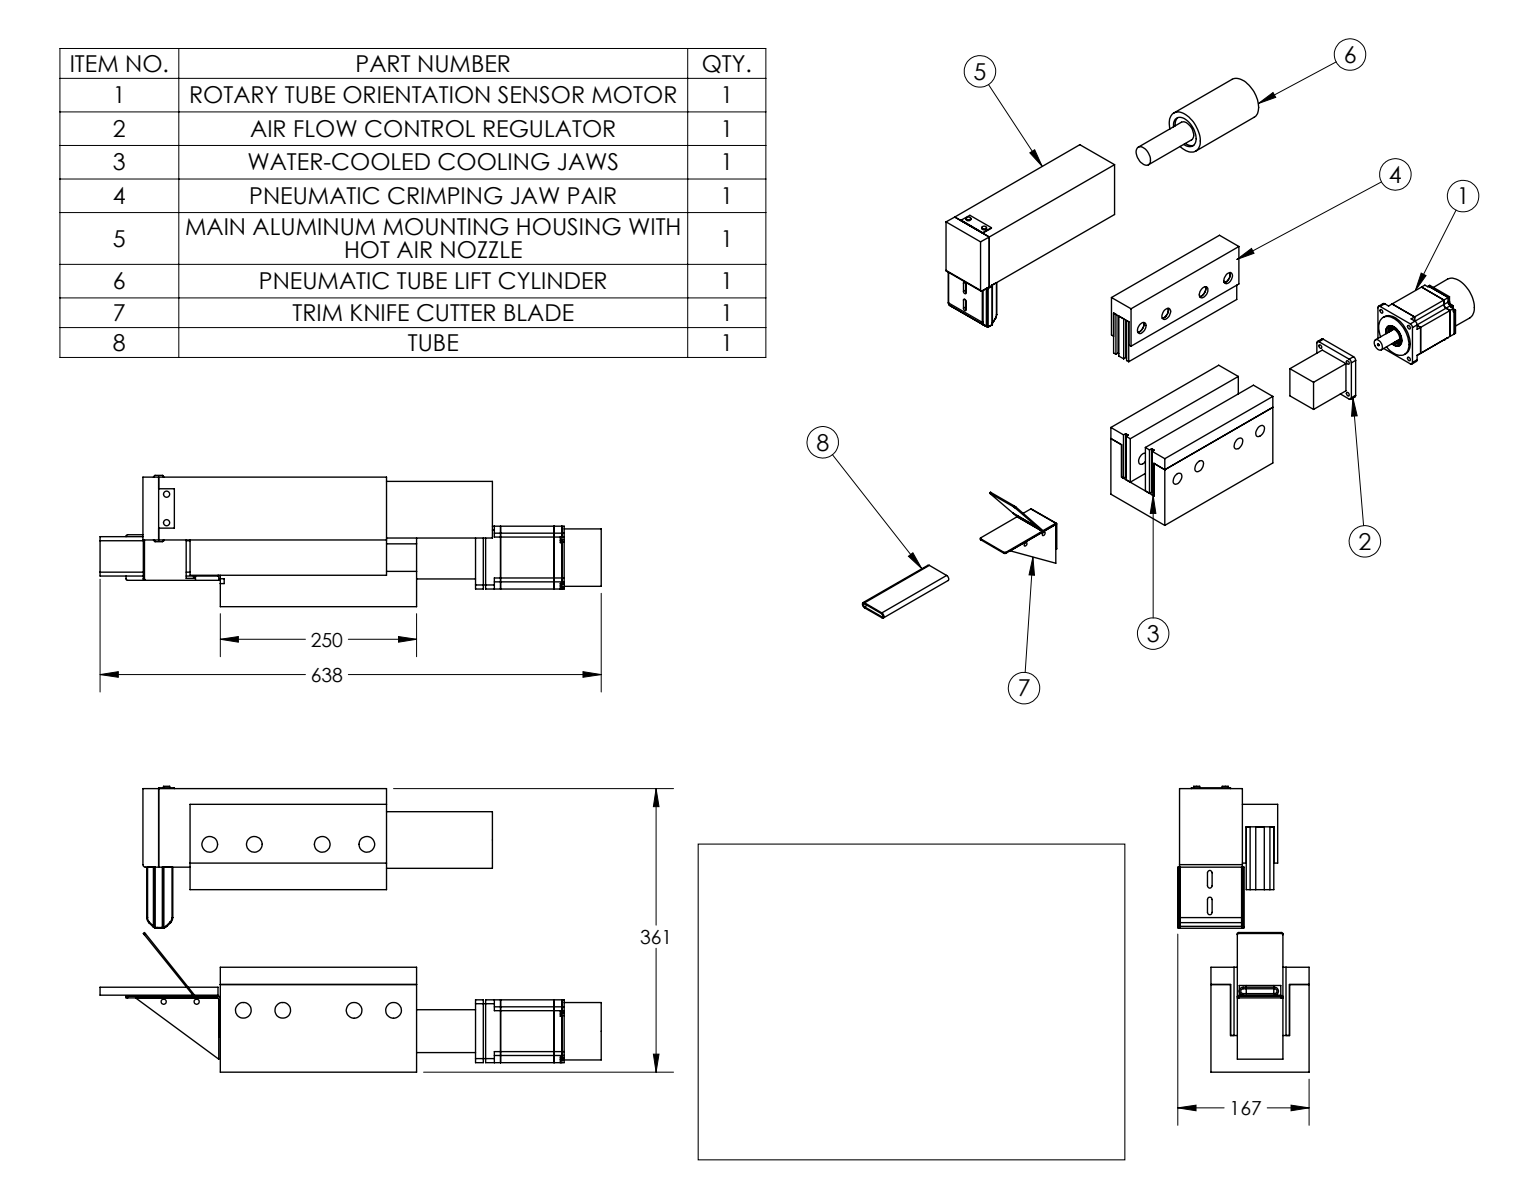
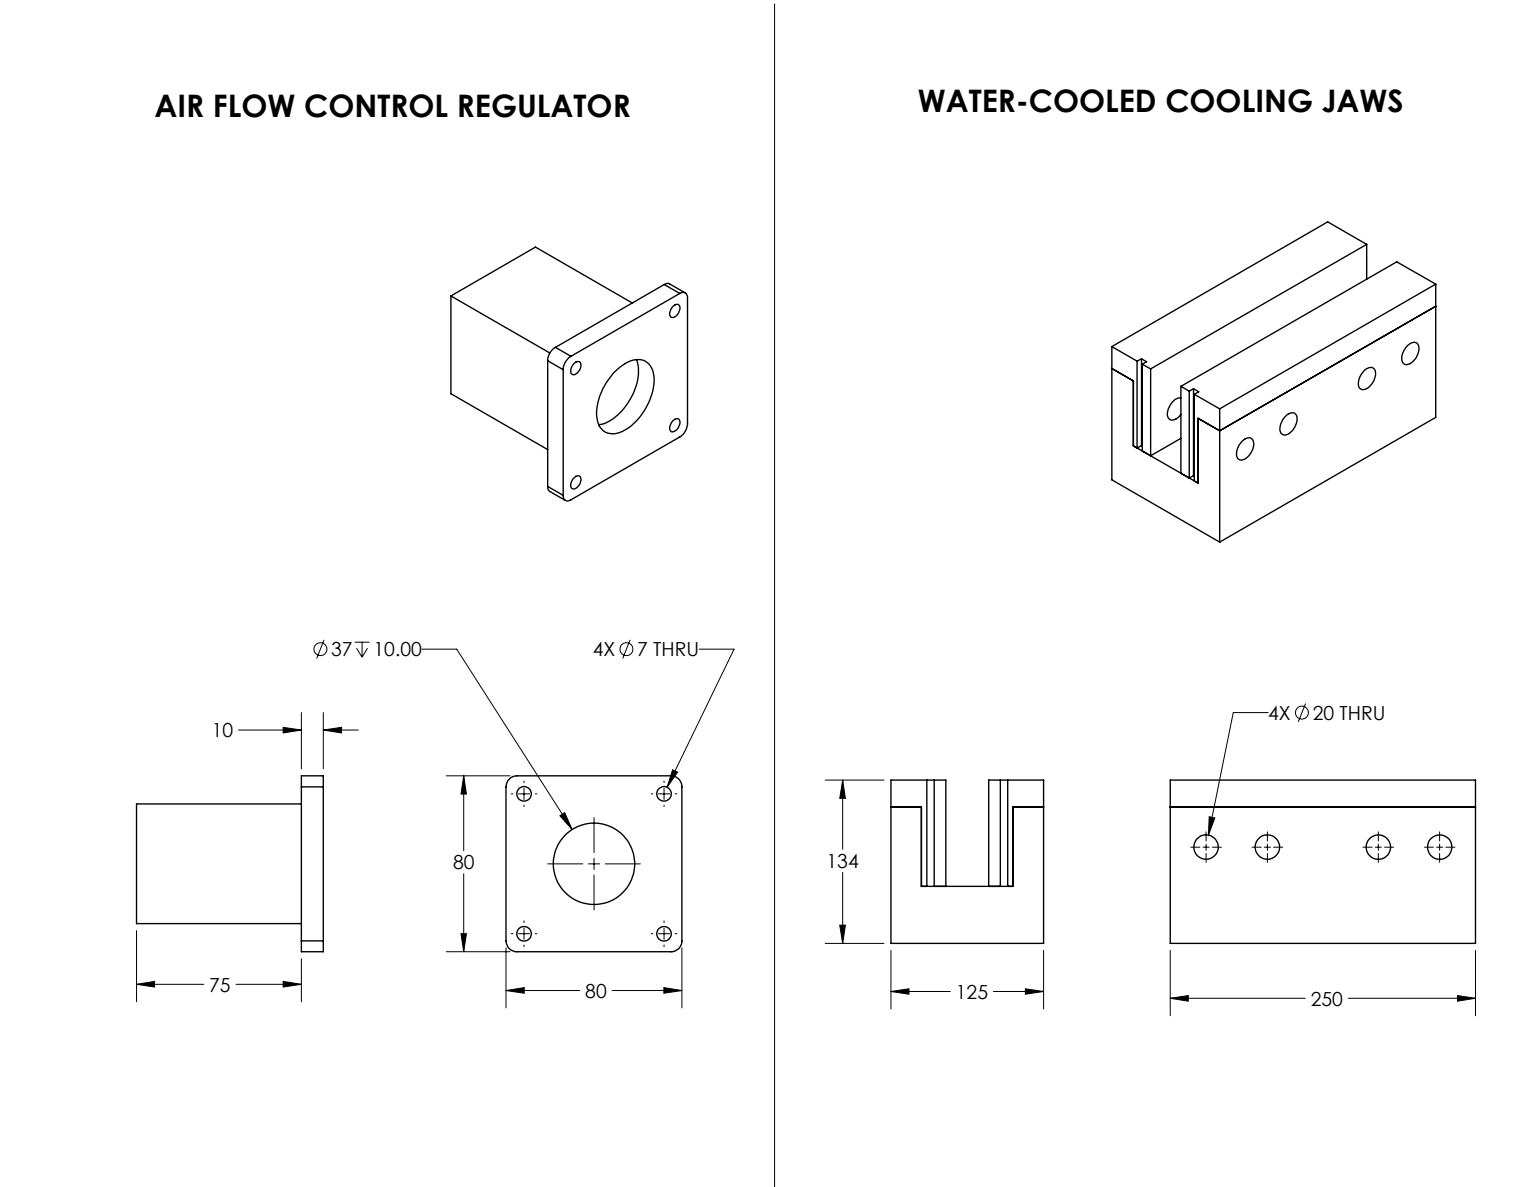
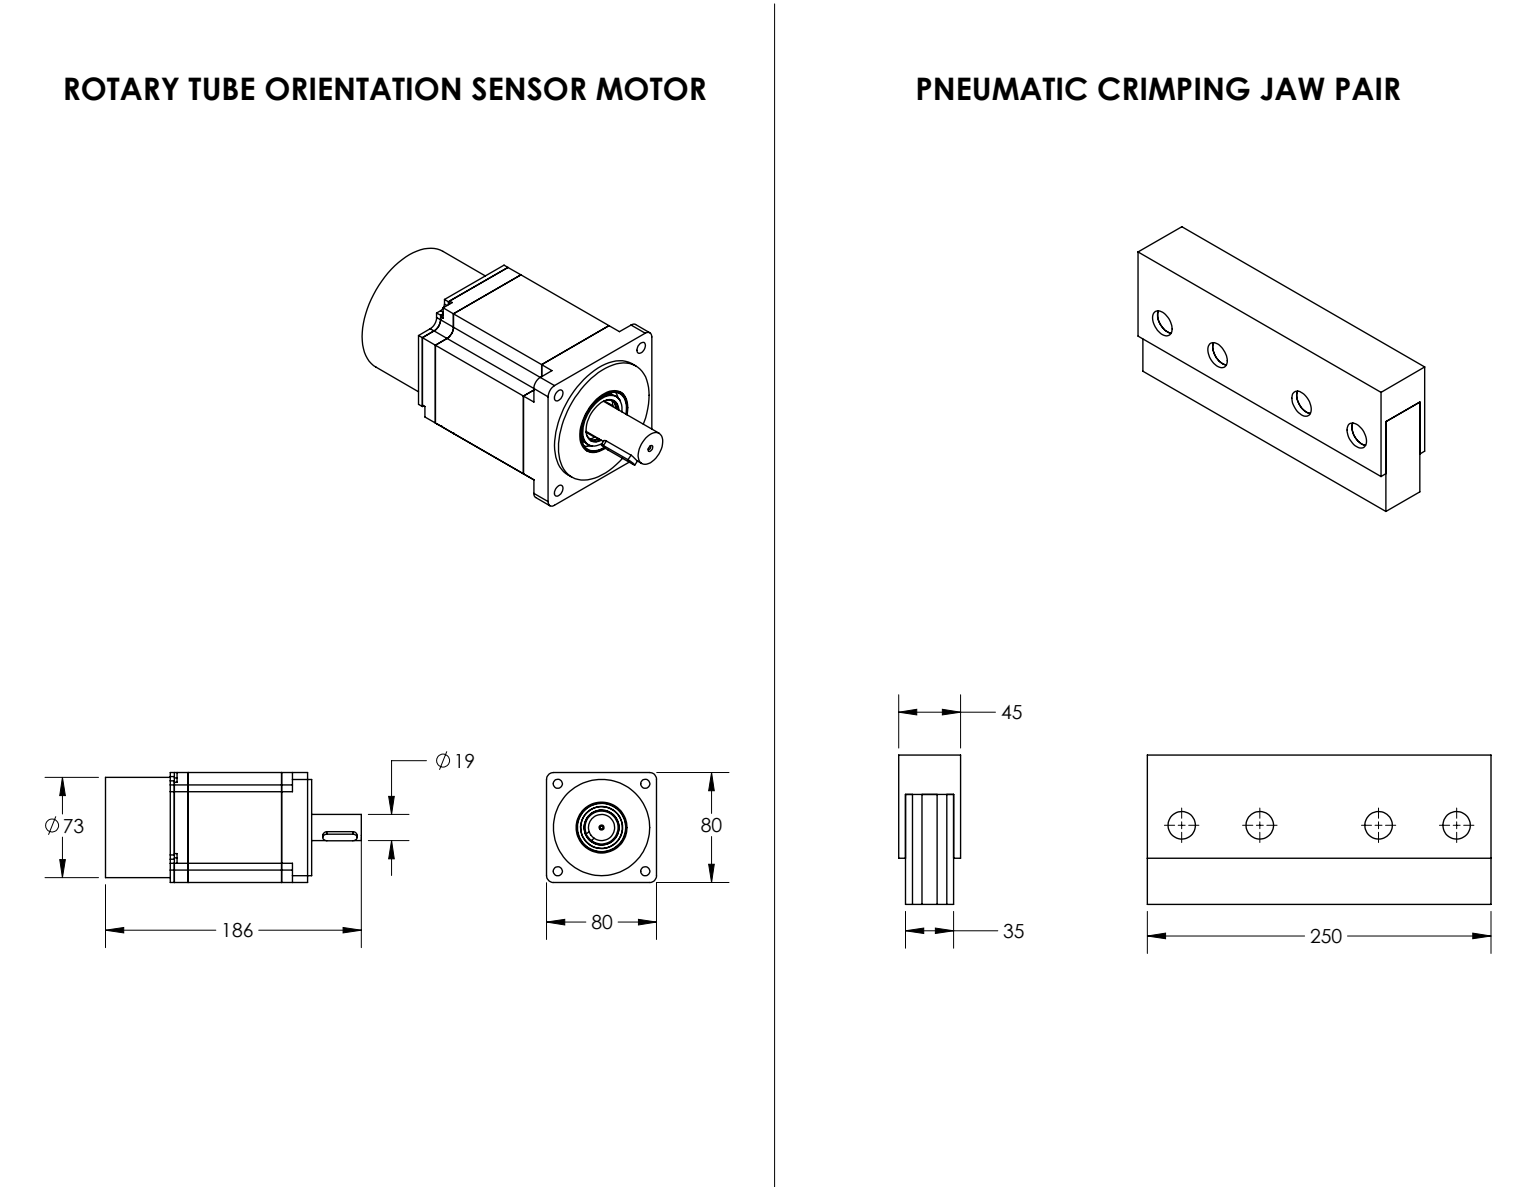
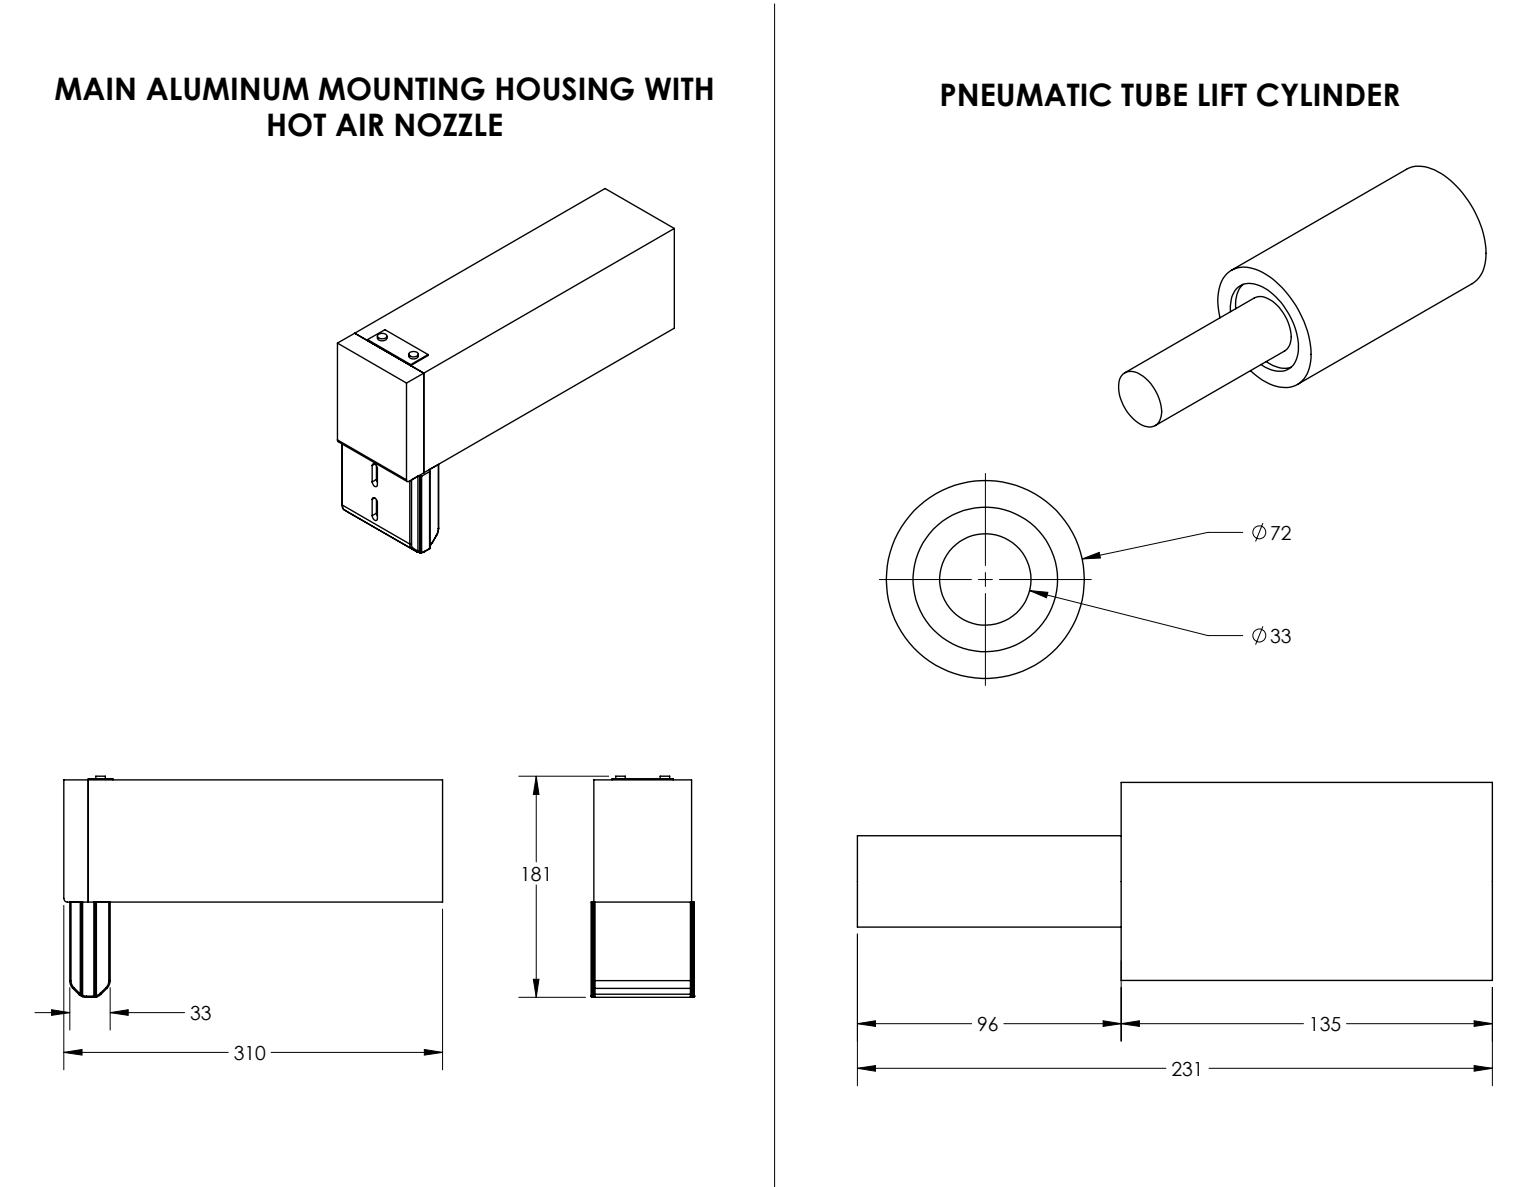
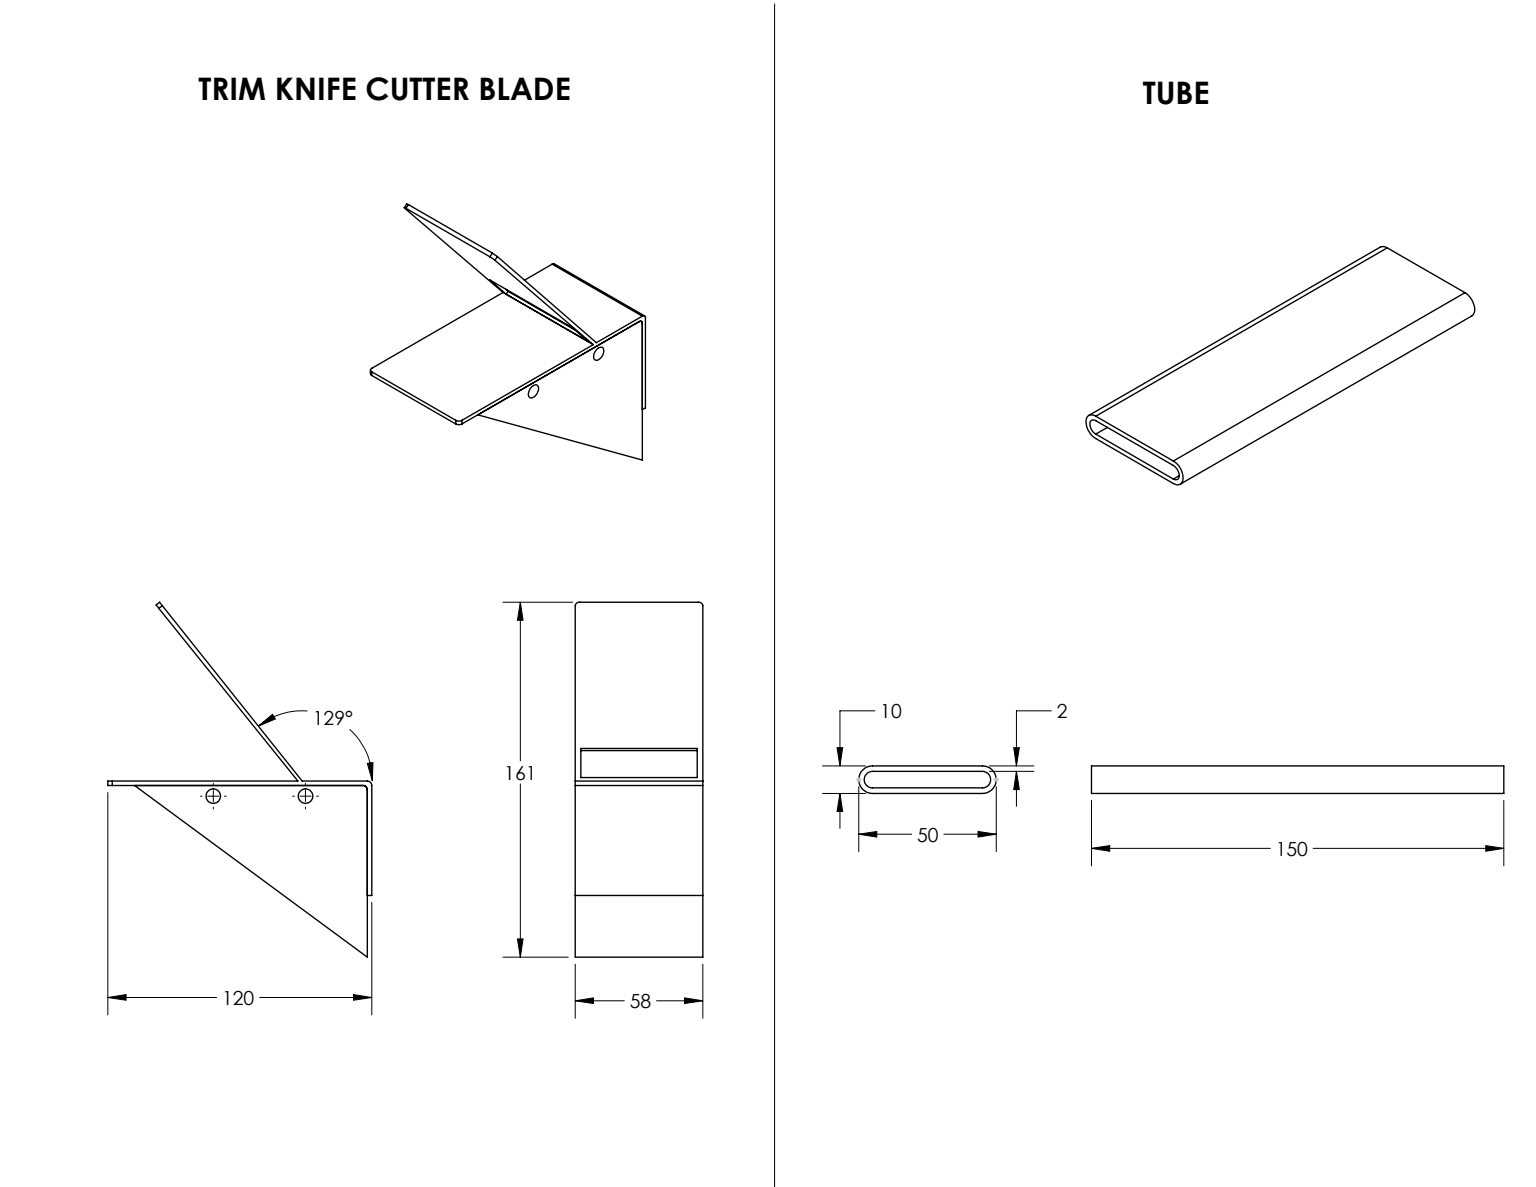
ISO-10303-21;
HEADER;
FILE_DESCRIPTION (('STEP AP214'),
    '1' );
FILE_NAME ('TAS-006',
    '2026-11-01T06:29:40',
    ( '' ),
    ( '' ),
    'SwSTEP 2.0',
    'SolidWorks 2024',
    '' );
FILE_SCHEMA (( 'AUTOMOTIVE_DESIGN' ));
ENDSEC;

DATA;
#1 = DIRECTION ( 'NONE',  ( -1.000000000000000000, 0.000000000000000000, 0.000000000000000000 ) ) ;
#2 = VECTOR ( 'NONE', #10690, 1000.000000000000000 ) ;
#3 = CARTESIAN_POINT ( 'NONE',  ( 26.00000000000000000, 19.00000000000000000, 40.00000000000001421 ) ) ;
#4 = VECTOR ( 'NONE', #1061, 1000.000000000000227 ) ;
#5 = SURFACE_STYLE_USAGE ( .BOTH. , #14117 ) ;
#6 = AXIS2_PLACEMENT_3D ( 'NONE', #11999, #10445, #9105 ) ;
#7 = DIRECTION ( 'NONE',  ( -0.000000000000000000, -0.000000000000000000, 1.000000000000000000 ) ) ;
#8 = FACE_OUTER_BOUND ( 'NONE', #1374, .T. ) ;
#9 = CARTESIAN_POINT ( 'NONE',  ( -0.9675204218459506622, 140.4913968989433499, 501.9874629796761383 ) ) ;
#10 = EDGE_CURVE ( 'NONE', #8032, #20154, #10638, .T. ) ;
#11 = ORIENTED_EDGE ( 'NONE', *, *, #4617, .F. ) ;
#12 = CARTESIAN_POINT ( 'NONE',  ( 153.4893729001366580, 145.9162550801369491, 0.000000000000000000 ) ) ;
#13 = CARTESIAN_POINT ( 'NONE',  ( 498.8334540492693918, 191.8198460455371333, 24.99421986894476078 ) ) ;
#14 = VECTOR ( 'NONE', #3072, 1000.000000000000000 ) ;
#15 = VECTOR ( 'NONE', #3910, 1000.000000000000000 ) ;
#16 = ORIENTED_EDGE ( 'NONE', *, *, #4980, .F. ) ;
#17 = DIRECTION ( 'NONE',  ( 0.000000000000000000, 1.000000000000000000, 0.000000000000000000 ) ) ;
#18 = ORIENTED_EDGE ( 'NONE', *, *, #2305, .F. ) ;
#19 = ADVANCED_FACE ( 'NONE', ( #19045 ), #8159, .F. ) ;
#20 = LINE ( 'NONE', #3221, #19065 ) ;
#21 = VERTEX_POINT ( 'NONE', #6304 ) ;
#22 = DIRECTION ( 'NONE',  ( 6.123031769111888756E-17, -1.000000000000000000, -3.749151804555344967E-33 ) ) ;
#23 = CARTESIAN_POINT ( 'NONE',  ( 143.0892156028631348, 80.91625508013694912, 245.0000000000000000 ) ) ;
#24 = CARTESIAN_POINT ( 'NONE',  ( -79.99999999999995737, 146.1184945051221575, 507.7561228916242158 ) ) ;
#25 = COLOUR_RGB ( '', 0.66274510, 0.83137255, 0.94901961) ;
#26 = CARTESIAN_POINT ( 'NONE',  ( 0.7168072523057583689, 140.4381783004008355, 500.8620105408696759 ) ) ;
#27 = STYLED_ITEM ( 'NONE', ( #13030 ), #7501 ) ;
#28 = CARTESIAN_POINT ( 'NONE',  ( -20.99999999999999645, 19.00000000000000000, -35.00000000000000711 ) ) ;
#29 = FACE_OUTER_BOUND ( 'NONE', #7471, .T. ) ;
#30 = EDGE_LOOP ( 'NONE', ( #17884, #17618, #18763, #13200 ) ) ;
#31 = FACE_OUTER_BOUND ( 'NONE', #2574, .T. ) ;
#32 = CARTESIAN_POINT ( 'NONE',  ( -211.5106270998635409, 123.1299228374912644, 29.36128450348865471 ) ) ;
#33 = SURFACE_STYLE_FILL_AREA ( #7869 ) ;
#34 = APPLICATION_PROTOCOL_DEFINITION ( 'draft international standard', 'automotive_design', 1998, #14741 ) ;
#35 = ADVANCED_FACE ( 'NONE', ( #14430 ), #12479, .F. ) ;
#36 = VERTEX_POINT ( 'NONE', #2241 ) ;
#37 = DIRECTION ( 'NONE',  ( 1.450371633464475582E-15, 0.000000000000000000, 1.000000000000000000 ) ) ;
#38 = ORIENTED_EDGE ( 'NONE', *, *, #17930, .F. ) ;
#39 = VERTEX_POINT ( 'NONE', #2353 ) ;
#40 = EDGE_CURVE ( 'NONE', #2779, #1878, #16207, .T. ) ;
#41 = ORIENTED_EDGE ( 'NONE', *, *, #2145, .F. ) ;
#42 = AXIS2_PLACEMENT_3D ( 'NONE', #8950, #992, #1291 ) ;
#43 = FACE_OUTER_BOUND ( 'NONE', #9378, .T. ) ;
#44 = ORIENTED_EDGE ( 'NONE', *, *, #9394, .T. ) ;
#45 = CARTESIAN_POINT ( 'NONE',  ( -18.00000000000001421, 10.00000000000000000, 36.00000000000000711 ) ) ;
#46 = ORIENTED_EDGE ( 'NONE', *, *, #5718, .T. ) ;
#47 = ADVANCED_FACE ( 'NONE', ( #11337 ), #8253, .T. ) ;
#48 = LINE ( 'NONE', #1353, #17512 ) ;
#49 = EDGE_CURVE ( 'NONE', #6461, #198, #5065, .T. ) ;
#50 = CARTESIAN_POINT ( 'NONE',  ( -80.02029401320167779, 140.0128597322520250, 488.8018784672104289 ) ) ;
#51 = LINE ( 'NONE', #155, #16644 ) ;
#52 = PRESENTATION_STYLE_ASSIGNMENT (( #17370 ) ) ;
#53 = VERTEX_POINT ( 'NONE', #1936 ) ;
#54 = PLANE ( 'NONE',  #1356 ) ;
#55 = LINE ( 'NONE', #6674, #3407 ) ;
#56 = DIRECTION ( 'NONE',  ( 1.000000000000000000, 0.000000000000000000, 0.000000000000000000 ) ) ;
#57 = DIRECTION ( 'NONE',  ( -1.000000000000000000, 0.000000000000000000, 0.000000000000000000 ) ) ;
#58 = ADVANCED_FACE ( 'NONE', ( #14835 ), #17880, .T. ) ;
#59 = CARTESIAN_POINT ( 'NONE',  ( 1.000000000002633005, 138.7723821175183048, 490.5025619656410640 ) ) ;
#60 = VECTOR ( 'NONE', #12496, 1000.000000000000000 ) ;
#61 = ORIENTED_EDGE ( 'NONE', *, *, #40, .F. ) ;
#62 = EDGE_CURVE ( 'NONE', #13882, #666, #19278, .T. ) ;
#63 = VERTEX_POINT ( 'NONE', #6718 ) ;
#64 = VECTOR ( 'NONE', #17487, 1000.000000000000000 ) ;
#65 = CARTESIAN_POINT ( 'NONE',  ( -80.34799141162025649, 140.6284191703059037, 501.0624196837977138 ) ) ;
#66 = COLOUR_RGB ( '', 0.40784314, 0.44705882, 0.49803922) ;
#67 = ORIENTED_EDGE ( 'NONE', *, *, #2522, .F. ) ;
#68 = EDGE_CURVE ( 'NONE', #13953, #12573, #6706, .T. ) ;
#69 = FILL_AREA_STYLE_COLOUR ( '', #11687 ) ;
#70 = DIRECTION ( 'NONE',  ( 1.000000000000000000, 5.889072920838430686E-16, -0.000000000000000000 ) ) ;
#71 = STYLED_ITEM ( 'NONE', ( #20272 ), #8119 ) ;
#72 = VERTEX_POINT ( 'NONE', #9896 ) ;
#73 = CARTESIAN_POINT ( 'NONE',  ( 0.000000000000000000, 65.20000000000000284, -5.741599279633704455E-16 ) ) ;
#74 = LINE ( 'NONE', #11013, #15228 ) ;
#75 = SURFACE_STYLE_FILL_AREA ( #19257 ) ;
#76 = AXIS2_PLACEMENT_3D ( 'NONE', #6689, #11306, #1507 ) ;
#77 = DIRECTION ( 'NONE',  ( 0.000000000000000000, 1.000000000000000000, 0.000000000000000000 ) ) ;
#78 = CARTESIAN_POINT ( 'NONE',  ( 37.00000000000000000, 0.000000000000000000, -23.00000000000000000 ) ) ;
#79 = DIRECTION ( 'NONE',  ( -0.000000000000000000, -1.000000000000000000, 0.000000000000000000 ) ) ;
#80 = DIRECTION ( 'NONE',  ( 0.000000000000000000, -7.137148015447440312E-15, 1.000000000000000000 ) ) ;
#81 = CIRCLE ( 'NONE', #4367, 34.00000000000000000 ) ;
#82 = COLOUR_RGB ( '', 0.40784314, 0.44705882, 0.49803922) ;
#83 = DIRECTION ( 'NONE',  ( 0.000000000000000000, 0.000000000000000000, 1.000000000000000000 ) ) ;
#84 = AXIS2_PLACEMENT_3D ( 'NONE', #6043, #6351, #15948 ) ;
#85 = EDGE_CURVE ( 'NONE', #13473, #6022, #2032, .T. ) ;
#86 = EDGE_LOOP ( 'NONE', ( #9308, #6599, #8630, #2907 ) ) ;
#87 = ORIENTED_EDGE ( 'NONE', *, *, #10548, .T. ) ;
#88 = UNCERTAINTY_MEASURE_WITH_UNIT (LENGTH_MEASURE( 1.000000000000000082E-05 ), #2098, 'distance_accuracy_value', 'NONE');
#89 = VECTOR ( 'NONE', #7, 1000.000000000000000 ) ;
#90 = ORIENTED_EDGE ( 'NONE', *, *, #8211, .T. ) ;
#91 = EDGE_LOOP ( 'NONE', ( #10928, #13194, #595, #9190 ) ) ;
#92 = EDGE_CURVE ( 'NONE', #18509, #14793, #2739, .T. ) ;
#93 = ORIENTED_EDGE ( 'NONE', *, *, #12996, .T. ) ;
#94 = LINE ( 'NONE', #202, #3499 ) ;
#95 = LINE ( 'NONE', #3199, #3080 ) ;
#96 = AXIS2_PLACEMENT_3D ( 'NONE', #6104, #4649, #10939 ) ;
#97 = MECHANICAL_DESIGN_GEOMETRIC_PRESENTATION_REPRESENTATION (  '', ( #748 ), #10965 ) ;
#98 = DIRECTION ( 'NONE',  ( 0.000000000000000000, 0.000000000000000000, -1.000000000000000000 ) ) ;
#99 = LINE ( 'NONE', #6410, #14355 ) ;
#100 = ORIENTED_EDGE ( 'NONE', *, *, #10783, .T. ) ;
#101 = CARTESIAN_POINT ( 'NONE',  ( 4.025000000000000355, 0.000000000000000000, 0.000000000000000000 ) ) ;
#102 = FACE_OUTER_BOUND ( 'NONE', #1105, .T. ) ;
#103 = PRESENTATION_STYLE_ASSIGNMENT (( #12482 ) ) ;
#104 = SURFACE_STYLE_USAGE ( .BOTH. , #15704 ) ;
#105 = DIRECTION ( 'NONE',  ( -1.000000000000000000, -1.595148023886719315E-16, 0.000000000000000000 ) ) ;
#106 = VECTOR ( 'NONE', #515, 1000.000000000000000 ) ;
#107 = ORIENTED_EDGE ( 'NONE', *, *, #6001, .T. ) ;
#108 = CARTESIAN_POINT ( 'NONE',  ( 1.181929469892980755, 138.7545334744432637, 496.6642397995875058 ) ) ;
#109 = CARTESIAN_POINT ( 'NONE',  ( -211.5106270998635409, 113.1299228374912502, 170.4174721992565082 ) ) ;
#110 = COLOUR_RGB ( '', 0.40784314, 0.44705882, 0.49803922) ;
#111 = AXIS2_PLACEMENT_3D ( 'NONE', #18474, #20009, #10456 ) ;
#112 = VECTOR ( 'NONE', #11852, 1000.000000000000000 ) ;
#113 = ORIENTED_EDGE ( 'NONE', *, *, #3039, .T. ) ;
#114 = COLOUR_RGB ( '', 0.72549020, 0.75294118, 0.79215686) ;
#115 = EDGE_CURVE ( 'NONE', #7815, #10453, #9998, .T. ) ;
#116 = FACE_OUTER_BOUND ( 'NONE', #6179, .T. ) ;
#117 = ORIENTED_EDGE ( 'NONE', *, *, #15149, .T. ) ;
#118 = ORIENTED_EDGE ( 'NONE', *, *, #16621, .F. ) ;
#119 = CARTESIAN_POINT ( 'NONE',  ( -36.00000000000000711, 8.000000000000000000, -19.00000000000000000 ) ) ;
#120 = CYLINDRICAL_SURFACE ( 'NONE', #15953, 8.000000000000000000 ) ;
#121 = PRESENTATION_STYLE_ASSIGNMENT (( #11153 ) ) ;
#122 = CIRCLE ( 'NONE', #10382, 4.999999999999997335 ) ;
#123 = CARTESIAN_POINT ( 'NONE',  ( 0.5497658814424238871, 139.8002724027203101, 500.9202994310167014 ) ) ;
#124 = CARTESIAN_POINT ( 'NONE',  ( 463.8334540492693350, 214.2156642432025251, 250.0000000000000000 ) ) ;
#125 = DIRECTION ( 'NONE',  ( -1.156482317317881191E-15, 0.000000000000000000, -1.000000000000000000 ) ) ;
#126 = AXIS2_PLACEMENT_3D ( 'NONE', #3364, #17466, #11787 ) ;
#127 = CARTESIAN_POINT ( 'NONE',  ( -34.99999999999998579, 3.000000000000000000, 21.00000000000000355 ) ) ;
#128 = ORIENTED_EDGE ( 'NONE', *, *, #4695, .T. ) ;
#129 = CARTESIAN_POINT ( 'NONE',  ( 88.88953019741013861, 80.91625508013694912, 250.0000000000000000 ) ) ;
#130 = DIRECTION ( 'NONE',  ( 0.000000000000000000, -0.000000000000000000, 1.000000000000000000 ) ) ;
#131 = DIRECTION ( 'NONE',  ( -1.000000000000000000, 0.000000000000000000, -0.000000000000000000 ) ) ;
#132 = SHAPE_DEFINITION_REPRESENTATION ( #9089, #16597 ) ;
#133 = VECTOR ( 'NONE', #9166, 1000.000000000000000 ) ;
#134 = CIRCLE ( 'NONE', #15629, 3.883636366625808911 ) ;
#135 = DIRECTION ( 'NONE',  ( -1.000000000000000000, -0.000000000000000000, -0.000000000000000000 ) ) ;
#136 = ORIENTED_EDGE ( 'NONE', *, *, #16204, .F. ) ;
#137 = AXIS2_PLACEMENT_3D ( 'NONE', #11998, #18269, #4176 ) ;
#138 = ADVANCED_FACE ( 'NONE', ( #10496 ), #19962, .F. ) ;
#139 = ORIENTED_EDGE ( 'NONE', *, *, #1969, .T. ) ;
#140 = VERTEX_POINT ( 'NONE', #7427 ) ;
#141 = AXIS2_PLACEMENT_3D ( 'NONE', #16061, #16163, #8419 ) ;
#142 = AXIS2_PLACEMENT_3D ( 'NONE', #2894, #15492, #7757 ) ;
#143 = AXIS2_PLACEMENT_3D ( 'NONE', #8052, #14338, #11231 ) ;
#144 = FACE_OUTER_BOUND ( 'NONE', #3451, .T. ) ;
#145 = CIRCLE ( 'NONE', #2460, 10.00000000000000888 ) ;
#146 = ORIENTED_EDGE ( 'NONE', *, *, #12401, .F. ) ;
#147 = EDGE_LOOP ( 'NONE', ( #13089, #906, #3735 ) ) ;
#148 = DIRECTION ( 'NONE',  ( 1.000000000000000000, -0.000000000000000000, -0.000000000000000000 ) ) ;
#149 = AXIS2_PLACEMENT_3D ( 'NONE', #4026, #19876, #8780 ) ;
#150 = EDGE_CURVE ( 'NONE', #4273, #9122, #5658, .T. ) ;
#151 = SURFACE_STYLE_USAGE ( .BOTH. , #18792 ) ;
#152 = VECTOR ( 'NONE', #13179, 1000.000000000000000 ) ;
#153 = CARTESIAN_POINT ( 'NONE',  ( -31.00000000000005684, 10.00000000000000000, -23.00000000000000000 ) ) ;
#154 = CARTESIAN_POINT ( 'NONE',  ( -22.99999999999999645, 68.00000000000000000, -36.99999999999999289 ) ) ;
#155 = CARTESIAN_POINT ( 'NONE',  ( 111.4893729001366012, 129.7247684487574588, 370.0000000000000000 ) ) ;
#156 = FILL_AREA_STYLE_COLOUR ( '', #13786 ) ;
#157 = FACE_OUTER_BOUND ( 'NONE', #9168, .T. ) ;
#158 = PRODUCT_DEFINITION ( 'UNKNOWN', '', #17864, #596 ) ;
#159 = VERTEX_POINT ( 'NONE', #897 ) ;
#160 = CYLINDRICAL_SURFACE ( 'NONE', #19995, 3.000000000000002665 ) ;
#161 = AXIS2_PLACEMENT_3D ( 'NONE', #2517, #8811, #5420 ) ;
#162 = CARTESIAN_POINT ( 'NONE',  ( -80.99999999999995737, 216.7545334744432921, 500.8237260975782874 ) ) ;
#163 = DIRECTION ( 'NONE',  ( 0.000000000000000000, -1.000000000000000000, 0.000000000000000000 ) ) ;
#164 = DIRECTION ( 'NONE',  ( 1.000000000000000000, 5.889072920838430686E-16, 0.000000000000000000 ) ) ;
#165 = PRESENTATION_STYLE_ASSIGNMENT (( #8000 ) ) ;
#166 = CARTESIAN_POINT ( 'NONE',  ( 22.99999999999998224, 0.000000000000000000, -31.00000000000003197 ) ) ;
#167 = CIRCLE ( 'NONE', #19893, 10.00000000000001066 ) ;
#168 = DIRECTION ( 'NONE',  ( 0.000000000000000000, 1.000000000000000000, 0.000000000000000000 ) ) ;
#169 = FACE_OUTER_BOUND ( 'NONE', #20181, .T. ) ;
#170 = ADVANCED_FACE ( 'NONE', ( #11955 ), #17305, .F. ) ;
#171 = ORIENTED_EDGE ( 'NONE', *, *, #8727, .T. ) ;
#172 = PRESENTATION_LAYER_ASSIGNMENT (  '', '', ( #19558 ) ) ;
#173 = EDGE_CURVE ( 'NONE', #9315, #975, #7926, .T. ) ;
#174 = B_SPLINE_CURVE_WITH_KNOTS ( 'NONE', 3,
 ( #18997, #9526, #1676, #11279, #9328, #17269, #7796, #50, #14073, #6556 ),
 .UNSPECIFIED., .F., .F.,
 ( 4, 2, 2, 2, 4 ),
 ( 0.000000000000000000, 0.0004092867322129563616, 0.0008185734644259127233, 0.001227860196638869139, 0.001637146928851825447 ),
 .UNSPECIFIED. ) ;
#175 = ORIENTED_EDGE ( 'NONE', *, *, #16048, .T. ) ;
#176 = SURFACE_STYLE_FILL_AREA ( #14295 ) ;
#177 = CARTESIAN_POINT ( 'NONE',  ( -79.93109621574201640, 140.7262008160015796, 502.2906755942678956 ) ) ;
#178 = EDGE_LOOP ( 'NONE', ( #2107, #7086, #9051, #14398 ) ) ;
#179 = CARTESIAN_POINT ( 'NONE',  ( 22.99999999999995737, 3.000000000000000000, -36.99999999999999289 ) ) ;
#180 = AXIS2_PLACEMENT_3D ( 'NONE', #5824, #8901, #12102 ) ;
#181 = EDGE_CURVE ( 'NONE', #5834, #20212, #6394, .T. ) ;
#182 = CYLINDRICAL_SURFACE ( 'NONE', #18527, 10.00000000000000888 ) ;
#183 = VERTEX_POINT ( 'NONE', #9617 ) ;
#184 = DIRECTION ( 'NONE',  ( 0.000000000000000000, 0.000000000000000000, 1.000000000000000000 ) ) ;
#185 = LINE ( 'NONE', #15988, #394 ) ;
#186 = VECTOR ( 'NONE', #8676, 1000.000000000000000 ) ;
#187 = EDGE_CURVE ( 'NONE', #8093, #1892, #19205, .T. ) ;
#188 = CARTESIAN_POINT ( 'NONE',  ( 39.99999999999999289, 0.000000000000000000, 26.00000000000000000 ) ) ;
#189 = CIRCLE ( 'NONE', #15696, 2.000000000000001776 ) ;
#190 = CARTESIAN_POINT ( 'NONE',  ( 31.00000000000001421, 10.00000000000000000, 22.99999999999999645 ) ) ;
#191 = DIRECTION ( 'NONE',  ( 1.000000000000000000, 0.000000000000000000, 0.000000000000000000 ) ) ;
#192 = ADVANCED_FACE ( 'NONE', ( #16149 ), #14568, .F. ) ;
#193 = CARTESIAN_POINT ( 'NONE',  ( 53.48937290013657986, 209.1356689931817243, 347.4957642363283412 ) ) ;
#194 = DIRECTION ( 'NONE',  ( -1.000000000000000000, -0.000000000000000000, -0.000000000000000000 ) ) ;
#195 = CARTESIAN_POINT ( 'NONE',  ( -3.000000000000000000, -1.836909530733565148E-16, 22.00000000000000000 ) ) ;
#196 = EDGE_CURVE ( 'NONE', #14622, #5083, #17893, .T. ) ;
#197 = ORIENTED_EDGE ( 'NONE', *, *, #17192, .T. ) ;
#198 = VERTEX_POINT ( 'NONE', #11872 ) ;
#199 = ORIENTED_EDGE ( 'NONE', *, *, #12617, .F. ) ;
#200 = ORIENTED_EDGE ( 'NONE', *, *, #10989, .T. ) ;
#201 = ORIENTED_EDGE ( 'NONE', *, *, #1906, .T. ) ;
#202 = CARTESIAN_POINT ( 'NONE',  ( 35.00000000000003553, -20.00000000000000000, -23.50000000000000000 ) ) ;
#203 = VECTOR ( 'NONE', #508, 1000.000000000000114 ) ;
#204 = SURFACE_STYLE_USAGE ( .BOTH. , #2043 ) ;
#205 = DIRECTION ( 'NONE',  ( 1.000000000000000000, 0.000000000000000000, 0.000000000000000000 ) ) ;
#206 = LINE ( 'NONE', #303, #6567 ) ;
#207 = CARTESIAN_POINT ( 'NONE',  ( 55.98937290013660828, 143.5567736071463401, 294.7336993003747239 ) ) ;
#208 = PRODUCT ( 'Servo-Axe', 'Servo-Axe', '', ( #17249 ) ) ;
#209 =( NAMED_UNIT ( * ) PLANE_ANGLE_UNIT ( ) SI_UNIT ( $, .RADIAN. ) );
#210 = DIRECTION ( 'NONE',  ( 6.123031769111888756E-17, 0.000000000000000000, 1.000000000000000000 ) ) ;
#211 = CARTESIAN_POINT ( 'NONE',  ( -78.99999999999995737, 216.7545334744432921, 509.3921618609452935 ) ) ;
#212 = LINE ( 'NONE', #17217, #9303 ) ;
#213 = SURFACE_SIDE_STYLE ('',( #11233 ) ) ;
#214 = ORIENTED_EDGE ( 'NONE', *, *, #11946, .T. ) ;
#215 = DIRECTION ( 'NONE',  ( -1.000000000000000000, -0.000000000000000000, -0.000000000000000000 ) ) ;
#216 = ADVANCED_FACE ( 'NONE', ( #1785 ), #8096, .F. ) ;
#217 = CARTESIAN_POINT ( 'NONE',  ( 78.48937290013660117, 103.1299228374914065, 79.58252780074349175 ) ) ;
#218 = VECTOR ( 'NONE', #4286, 1000.000000000000000 ) ;
#219 = ADVANCED_FACE ( 'NONE', ( #3459 ), #14966, .T. ) ;
#220 = EDGE_CURVE ( 'NONE', #6682, #1451, #10317, .T. ) ;
#221 = EDGE_LOOP ( 'NONE', ( #13172, #3840 ) ) ;
#222 = DIRECTION ( 'NONE',  ( -5.099857904826354583E-14, -0.3949357872488052368, -0.9187087263927380398 ) ) ;
#223 = EDGE_LOOP ( 'NONE', ( #20266, #17142, #2719, #16147, #10756, #6546, #7481, #19067, #9107, #14805, #17273, #15955 ) ) ;
#224 = ORIENTED_EDGE ( 'NONE', *, *, #18076, .T. ) ;
#225 = CARTESIAN_POINT ( 'NONE',  ( 0.000000000000000000, 10.00000000000000000, 0.000000000000000000 ) ) ;
#226 = PLANE ( 'NONE',  #3633 ) ;
#227 = ORIENTED_EDGE ( 'NONE', *, *, #4552, .F. ) ;
#228 = DIRECTION ( 'NONE',  ( 1.000000000000000000, -0.000000000000000000, 0.000000000000000000 ) ) ;
#229 = SURFACE_STYLE_USAGE ( .BOTH. , #1757 ) ;
#230 = CARTESIAN_POINT ( 'NONE',  ( 0.9999999999997754019, 139.4861549369088038, 500.2186618848269859 ) ) ;
#231 = CARTESIAN_POINT ( 'NONE',  ( 10.00000000000000000, 381.0487089519837127, -150.0000000000032685 ) ) ;
#232 = SURFACE_STYLE_FILL_AREA ( #12504 ) ;
#233 = B_SPLINE_CURVE_WITH_KNOTS ( 'NONE', 3,
 ( #2154, #5367, #12797, #3521, #9692, #8463, #14739, #9798, #14639, #306, #11544, #6719, #13012, #17724, #16110, #13117, #516, #14527 ),
 .UNSPECIFIED., .F., .F.,
 ( 4, 2, 2, 2, 2, 2, 2, 2, 4 ),
 ( 0.004721323624227211080, 0.005310725018217473184, 0.005900126412207735288, 0.006489527806197996525, 0.007078929200188269905, 0.007668330594178543284, 0.008257731988168816664, 0.008847133382159089177, 0.009436534776149363424 ),
 .UNSPECIFIED. ) ;
#234 = CARTESIAN_POINT ( 'NONE',  ( -211.5106270998635409, 113.1299228374912502, 79.58252780074349175 ) ) ;
#235 = ORIENTED_EDGE ( 'NONE', *, *, #11443, .F. ) ;
#236 = DIRECTION ( 'NONE',  ( 0.000000000000000000, -0.000000000000000000, 1.000000000000000000 ) ) ;
#237 = DIRECTION ( 'NONE',  ( 0.000000000000000000, 0.000000000000000000, 1.000000000000000000 ) ) ;
#238 = DIRECTION ( 'NONE',  ( 0.000000000000000000, 0.000000000000000000, -1.000000000000000000 ) ) ;
#239 = ADVANCED_FACE ( 'NONE', ( #10427 ), #20293, .T. ) ;
#240 = ORIENTED_EDGE ( 'NONE', *, *, #2391, .T. ) ;
#241 = AXIS2_PLACEMENT_3D ( 'NONE', #9899, #12700, #11340 ) ;
#242 = CARTESIAN_POINT ( 'NONE',  ( -22.99999999999999645, 0.000000000000000000, 37.00000000000002132 ) ) ;
#243 = VERTEX_POINT ( 'NONE', #16917 ) ;
#244 = ORIENTED_EDGE ( 'NONE', *, *, #4195, .F. ) ;
#245 = ORIENTED_EDGE ( 'NONE', *, *, #2016, .F. ) ;
#246 = SURFACE_SIDE_STYLE ('',( #6343 ) ) ;
#247 = DIRECTION ( 'NONE',  ( 1.000000000000000000, 0.000000000000000000, 0.000000000000000000 ) ) ;
#248 = EDGE_LOOP ( 'NONE', ( #19744, #15567 ) ) ;
#249 = AXIS2_PLACEMENT_3D ( 'NONE', #16527, #16428, #14757 ) ;
#250 = CARTESIAN_POINT ( 'NONE',  ( 178.4893729001365443, 145.9162550801369491, 0.000000000000000000 ) ) ;
#251 = DIRECTION ( 'NONE',  ( 1.000000000000000000, 0.000000000000000000, 0.000000000000000000 ) ) ;
#252 = DIRECTION ( 'NONE',  ( 1.000000000000000000, 0.000000000000000000, 1.135258727068399668E-15 ) ) ;
#253 = AXIS2_PLACEMENT_3D ( 'NONE', #6385, #12984, #18824 ) ;
#254 = SURFACE_STYLE_USAGE ( .BOTH. , #15843 ) ;
#255 = CARTESIAN_POINT ( 'NONE',  ( 178.4893729001365728, 113.1299228374914918, 79.58252780074349175 ) ) ;
#256 =( NAMED_UNIT ( * ) SI_UNIT ( $, .STERADIAN. ) SOLID_ANGLE_UNIT ( ) );
#257 = DIRECTION ( 'NONE',  ( 0.000000000000000000, 1.000000000000000000, -0.000000000000000000 ) ) ;
#258 = VERTEX_POINT ( 'NONE', #7740 ) ;
#259 =( NAMED_UNIT ( * ) PLANE_ANGLE_UNIT ( ) SI_UNIT ( $, .RADIAN. ) );
#260 = CARTESIAN_POINT ( 'NONE',  ( 39.99999999999999289, 10.00000000000000000, 18.99999999999999645 ) ) ;
#261 = SURFACE_STYLE_FILL_AREA ( #19230 ) ;
#262 = DIRECTION ( 'NONE',  ( 0.000000000000000000, 0.000000000000000000, -1.000000000000000000 ) ) ;
#263 =( NAMED_UNIT ( * ) SI_UNIT ( $, .STERADIAN. ) SOLID_ANGLE_UNIT ( ) );
#264 = DIRECTION ( 'NONE',  ( 6.123031769111888756E-17, -1.000000000000000000, -3.749151804555344967E-33 ) ) ;
#265 =( NAMED_UNIT ( * ) PLANE_ANGLE_UNIT ( ) SI_UNIT ( $, .RADIAN. ) );
#266 =( LENGTH_UNIT ( ) NAMED_UNIT ( * ) SI_UNIT ( .MILLI., .METRE. ) );
#267 = ORIENTED_EDGE ( 'NONE', *, *, #19357, .T. ) ;
#268 = VECTOR ( 'NONE', #14783, 1000.000000000000000 ) ;
#269 = ORIENTED_EDGE ( 'NONE', *, *, #15161, .F. ) ;
#270 = VERTEX_POINT ( 'NONE', #20189 ) ;
#271 = ORIENTED_EDGE ( 'NONE', *, *, #20336, .T. ) ;
#272 = PLANE ( 'NONE',  #1506 ) ;
#273 = EDGE_LOOP ( 'NONE', ( #888, #7387 ) ) ;
#274 = CARTESIAN_POINT ( 'NONE',  ( -77.99033078109007988, 125.7247684487574304, 252.0000000000000000 ) ) ;
#275 =( NAMED_UNIT ( * ) PLANE_ANGLE_UNIT ( ) SI_UNIT ( $, .RADIAN. ) );
#276 = ORIENTED_EDGE ( 'NONE', *, *, #9042, .F. ) ;
#277 = ADVANCED_FACE ( 'NONE', ( #7329 ), #10727, .F. ) ;
#278 = CARTESIAN_POINT ( 'NONE',  ( -26.00000000000002842, 3.000000000000000000, 31.00000000000003908 ) ) ;
#279 = DIRECTION ( 'NONE',  ( 9.815121534730717399E-17, -1.000000000000000000, 0.000000000000000000 ) ) ;
#280 = AXIS2_PLACEMENT_3D ( 'NONE', #12196, #10356, #7366 ) ;
#281 = CARTESIAN_POINT ( 'NONE',  ( 26.00000000000000000, 19.00000000000000000, 31.00000000000003197 ) ) ;
#282 = CARTESIAN_POINT ( 'NONE',  ( 7.000000000000000000, 17.85000000000000142, 0.000000000000000000 ) ) ;
#283 = FACE_BOUND ( 'NONE', #20284, .T. ) ;
#284 = CARTESIAN_POINT ( 'NONE',  ( 25.99999999999996092, 3.000000000000000000, -31.00000000000003197 ) ) ;
#285 = CARTESIAN_POINT ( 'NONE',  ( 78.48937290013660117, 113.1299228374914208, 170.4174721992565082 ) ) ;
#286 = LINE ( 'NONE', #7727, #4968 ) ;
#287 = ORIENTED_EDGE ( 'NONE', *, *, #15417, .F. ) ;
#288 = EDGE_CURVE ( 'NONE', #8097, #2140, #18654, .T. ) ;
#289 = ORIENTED_EDGE ( 'NONE', *, *, #3879, .T. ) ;
#290 = CIRCLE ( 'NONE', #19687, 10.00000000000001066 ) ;
#291 = ORIENTED_EDGE ( 'NONE', *, *, #15048, .F. ) ;
#292 = UNCERTAINTY_MEASURE_WITH_UNIT (LENGTH_MEASURE( 1.000000000000000082E-05 ), #17456, 'distance_accuracy_value', 'NONE');
#293 = COLOUR_RGB ( '', 0.31764706, 0.68627451, 0.89019608) ;
#294 = EDGE_CURVE ( 'NONE', #16045, #3349, #13619, .T. ) ;
#295 = CONICAL_SURFACE ( 'NONE', #19035, 13.89560290347679938, 1.567266246505109928 ) ;
#296 = VERTEX_POINT ( 'NONE', #2879 ) ;
#297 = ORIENTED_EDGE ( 'NONE', *, *, #12310, .T. ) ;
#298 = VERTEX_POINT ( 'NONE', #7631 ) ;
#299 = CARTESIAN_POINT ( 'NONE',  ( 5.425003271131650706, 0.000000000000000000, 0.000000000000000000 ) ) ;
#300 = EDGE_CURVE ( 'NONE', #18143, #9184, #13721, .T. ) ;
#301 = CARTESIAN_POINT ( 'NONE',  ( 39.99999999999999289, 10.00000000000000000, 26.00000000000000000 ) ) ;
#302 = CARTESIAN_POINT ( 'NONE',  ( 31.00000000000002842, 0.000000000000000000, 23.00000000000001066 ) ) ;
#303 = CARTESIAN_POINT ( 'NONE',  ( 153.4893729001366580, 0.000000000000000000, 250.0000000000000000 ) ) ;
#304 = DIRECTION ( 'NONE',  ( 0.000000000000000000, 0.000000000000000000, -1.000000000000000000 ) ) ;
#305 = VERTEX_POINT ( 'NONE', #6101 ) ;
#306 = CARTESIAN_POINT ( 'NONE',  ( 2.259918635623968441, 61.98265998586796854, 9.228371864727256124 ) ) ;
#307 = DIRECTION ( 'NONE',  ( -0.000000000000000000, -1.000000000000000000, -0.000000000000000000 ) ) ;
#308 = EDGE_CURVE ( 'NONE', #5039, #16269, #4244, .T. ) ;
#309 = MECHANICAL_DESIGN_GEOMETRIC_PRESENTATION_REPRESENTATION (  '', ( #4258 ), #18737 ) ;
#310 = AXIS2_PLACEMENT_3D ( 'NONE', #19605, #3865, #10144 ) ;
#311 = STYLED_ITEM ( 'NONE', ( #8924 ), #10883 ) ;
#312 = DIRECTION ( 'NONE',  ( -1.000000000000000000, 0.000000000000000000, 0.000000000000000000 ) ) ;
#313 = CARTESIAN_POINT ( 'NONE',  ( 178.4893729001365728, 123.1299228374914918, 170.4174721992565082 ) ) ;
#314 = EDGE_CURVE ( 'NONE', #4687, #4967, #10617, .T. ) ;
#315 = ORIENTED_EDGE ( 'NONE', *, *, #6787, .F. ) ;
#316 = EDGE_LOOP ( 'NONE', ( #20231, #12649, #16992, #19805 ) ) ;
#317 = EDGE_CURVE ( 'NONE', #19903, #10221, #2678, .T. ) ;
#318 = VECTOR ( 'NONE', #17699, 1000.000000000000000 ) ;
#319 = CIRCLE ( 'NONE', #2951, 4.999999999999997335 ) ;
#320 = DIRECTION ( 'NONE',  ( 1.000000000000000000, 5.889072920838430686E-16, -0.000000000000000000 ) ) ;
#321 = ORIENTED_EDGE ( 'NONE', *, *, #5960, .T. ) ;
#322 = CARTESIAN_POINT ( 'NONE',  ( 25.99999999999996092, 3.000000000000000000, 40.00000000000000711 ) ) ;
#323 = VERTEX_POINT ( 'NONE', #2782 ) ;
#324 = EDGE_CURVE ( 'NONE', #18810, #10116, #9084, .T. ) ;
#325 = CARTESIAN_POINT ( 'NONE',  ( 0.000000000000000000, 316.7545334744432353, 515.1946179577817020 ) ) ;
#326 = LINE ( 'NONE', #7046, #6763 ) ;
#327 = SURFACE_SIDE_STYLE ('',( #8181 ) ) ;
#328 = SURFACE_STYLE_FILL_AREA ( #17952 ) ;
#329 = CARTESIAN_POINT ( 'NONE',  ( -78.99999999999995737, 138.7545334744432637, 509.3921618609452935 ) ) ;
#330 = DIRECTION ( 'NONE',  ( 0.000000000000000000, 1.000000000000000000, -0.000000000000000000 ) ) ;
#331 = CARTESIAN_POINT ( 'NONE',  ( -64.99999999999995737, 316.7545334744432353, 495.1946179577816451 ) ) ;
#332 = DIRECTION ( 'NONE',  ( 0.000000000000000000, 0.000000000000000000, -1.000000000000000000 ) ) ;
#333 = ORIENTED_EDGE ( 'NONE', *, *, #2827, .F. ) ;
#334 = CARTESIAN_POINT ( 'NONE',  ( 486.8117674897343363, 134.2156642432025251, 245.0000000000000000 ) ) ;
#335 = FILL_AREA_STYLE ('',( #16240 ) ) ;
#336 = MECHANICAL_DESIGN_GEOMETRIC_PRESENTATION_REPRESENTATION (  '', ( #16173 ), #16815 ) ;
#337 = CONTEXT_DEPENDENT_SHAPE_REPRESENTATION ( #6721, #2821 ) ;
#338 = VECTOR ( 'NONE', #7157, 1000.000000000000227 ) ;
#339 =( GEOMETRIC_REPRESENTATION_CONTEXT ( 3 ) GLOBAL_UNCERTAINTY_ASSIGNED_CONTEXT ( ( #10174 ) ) GLOBAL_UNIT_ASSIGNED_CONTEXT ( ( #15376, #15481, #12696 ) ) REPRESENTATION_CONTEXT ( 'NONE', 'WORKASPACE' ) );
#340 = CARTESIAN_POINT ( 'NONE',  ( 26.00000000000000355, 19.00000000000000000, -31.00000000000003908 ) ) ;
#341 = ORIENTED_EDGE ( 'NONE', *, *, #5552, .F. ) ;
#342 = ORIENTED_EDGE ( 'NONE', *, *, #3625, .T. ) ;
#343 = ADVANCED_FACE ( 'NONE', ( #12380 ), #5984, .F. ) ;
#344 = ORIENTED_EDGE ( 'NONE', *, *, #1048, .F. ) ;
#345 = VERTEX_POINT ( 'NONE', #3296 ) ;
#346 = FACE_OUTER_BOUND ( 'NONE', #5460, .T. ) ;
#347 = ORIENTED_EDGE ( 'NONE', *, *, #7611, .T. ) ;
#348 = DIRECTION ( 'NONE',  ( 1.000000000000000000, 5.889072920838430686E-16, -0.000000000000000000 ) ) ;
#349 = PRESENTATION_LAYER_ASSIGNMENT (  '', '', ( #11208 ) ) ;
#350 = CARTESIAN_POINT ( 'NONE',  ( 0.01964375121925415052, 140.0139011465853685, 488.7997624681271418 ) ) ;
#351 = EDGE_LOOP ( 'NONE', ( #10484, #6293, #12449, #14964, #16000, #5547 ) ) ;
#352 = SURFACE_STYLE_USAGE ( .BOTH. , #14777 ) ;
#353 =( LENGTH_UNIT ( ) NAMED_UNIT ( * ) SI_UNIT ( .MILLI., .METRE. ) );
#354 = CARTESIAN_POINT ( 'NONE',  ( 37.00000000000000000, 68.00000000000000000, -23.00000000000000000 ) ) ;
#355 =( NAMED_UNIT ( * ) SI_UNIT ( $, .STERADIAN. ) SOLID_ANGLE_UNIT ( ) );
#356 = CARTESIAN_POINT ( 'NONE',  ( 31.81980515339464333, 11.00000000000000000, 28.51980515339463906 ) ) ;
#357 = ORIENTED_EDGE ( 'NONE', *, *, #6247, .F. ) ;
#358 = DIRECTION ( 'NONE',  ( 0.000000000000000000, 0.000000000000000000, -1.000000000000000000 ) ) ;
#359 = CARTESIAN_POINT ( 'NONE',  ( -3.000000000000002220, 60.00000000000000711, 6.000000000000000000 ) ) ;
#360 =( NAMED_UNIT ( * ) PLANE_ANGLE_UNIT ( ) SI_UNIT ( $, .RADIAN. ) );
#361 = LINE ( 'NONE', #16268, #1608 ) ;
#362 = ORIENTED_EDGE ( 'NONE', *, *, #20307, .T. ) ;
#363 = CIRCLE ( 'NONE', #17149, 3.300000000000011369 ) ;
#364 = ORIENTED_EDGE ( 'NONE', *, *, #8997, .T. ) ;
#365 = EDGE_LOOP ( 'NONE', ( #5974, #11325, #14847, #11434 ) ) ;
#366 = APPLICATION_CONTEXT ( 'automotive_design' ) ;
#367 = CARTESIAN_POINT ( 'NONE',  ( 25.99999999999996092, 3.000000000000000000, -31.00000000000003197 ) ) ;
#368 = VERTEX_POINT ( 'NONE', #3094 ) ;
#369 = LINE ( 'NONE', #19334, #12012 ) ;
#370 = EDGE_CURVE ( 'NONE', #3638, #20118, #95, .T. ) ;
#371 = CARTESIAN_POINT ( 'NONE',  ( 40.00000000000001421, 0.000000000000000000, -150.0000000000000000 ) ) ;
#372 = ORIENTED_EDGE ( 'NONE', *, *, #12021, .F. ) ;
#373 = CARTESIAN_POINT ( 'NONE',  ( -36.00000000000000711, 8.000000000000000000, -19.00000000000000000 ) ) ;
#374 = MECHANICAL_DESIGN_GEOMETRIC_PRESENTATION_REPRESENTATION (  '', ( #10253 ), #17163 ) ;
#375 = CARTESIAN_POINT ( 'NONE',  ( -3.795335389125381139E-15, 146.8256012863087960, 480.6843163258853906 ) ) ;
#376 = VECTOR ( 'NONE', #18670, 1000.000000000000000 ) ;
#377 = DIRECTION ( 'NONE',  ( -1.000000000000000000, 0.000000000000000000, 1.450371633464475582E-15 ) ) ;
#378 = DIRECTION ( 'NONE',  ( 1.000000000000000000, 9.815121534730717399E-17, -0.000000000000000000 ) ) ;
#379 = PLANE ( 'NONE',  #17601 ) ;
#380 = DIRECTION ( 'NONE',  ( 1.000000000000000000, -0.000000000000000000, 0.000000000000000000 ) ) ;
#381 = LINE ( 'NONE', #7755, #630 ) ;
#382 = DIRECTION ( 'NONE',  ( 0.000000000000000000, 0.000000000000000000, -1.000000000000000000 ) ) ;
#383 = PRESENTATION_STYLE_ASSIGNMENT (( #8528 ) ) ;
#384 = ORIENTED_EDGE ( 'NONE', *, *, #13185, .T. ) ;
#385 = EDGE_CURVE ( 'NONE', #13659, #12399, #1618, .T. ) ;
#386 = ORIENTED_EDGE ( 'NONE', *, *, #7319, .F. ) ;
#387 = COLOUR_RGB ( '', 0.72549020, 0.75294118, 0.79215686) ;
#388 = ORIENTED_EDGE ( 'NONE', *, *, #1932, .F. ) ;
#389 = VECTOR ( 'NONE', #583, 1000.000000000000000 ) ;
#390 = ORIENTED_EDGE ( 'NONE', *, *, #839, .F. ) ;
#391 = EDGE_LOOP ( 'NONE', ( #10090, #136, #7141, #4283 ) ) ;
#392 = DIRECTION ( 'NONE',  ( 0.000000000000000000, 0.000000000000000000, -1.000000000000000000 ) ) ;
#393 = DIRECTION ( 'NONE',  ( -1.000000000000000000, 0.000000000000000000, 0.000000000000000000 ) ) ;
#394 = VECTOR ( 'NONE', #20369, 1000.000000000000000 ) ;
#395 = FACE_OUTER_BOUND ( 'NONE', #6602, .T. ) ;
#396 = CARTESIAN_POINT ( 'NONE',  ( 35.00000000000000711, 8.000000000000000000, 35.00000000000000711 ) ) ;
#397 = CARTESIAN_POINT ( 'NONE',  ( -25.99999999999999645, 68.00000000000000000, -31.00000000000003197 ) ) ;
#399 = EDGE_CURVE ( 'NONE', #5413, #3192, #12898, .T. ) ;
#398 = FACE_BOUND ( 'NONE', #13239, .T. ) ;
#400 = CIRCLE ( 'NONE', #7646, 10.00000000000000888 ) ;
#401 = LINE ( 'NONE', #9484, #887 ) ;
#402 = AXIS2_PLACEMENT_3D ( 'NONE', #2225, #6812, #5247 ) ;
#403 = VECTOR ( 'NONE', #18306, 1000.000000000000000 ) ;
#404 = FACE_OUTER_BOUND ( 'NONE', #1206, .T. ) ;
#405 = CARTESIAN_POINT ( 'NONE',  ( 55.48937290013660117, 129.7247684487574588, 370.0000000000000000 ) ) ;
#406 = PRESENTATION_STYLE_ASSIGNMENT (( #19728 ) ) ;
#407 = EDGE_CURVE ( 'NONE', #6644, #18079, #6406, .T. ) ;
#408 = AXIS2_PLACEMENT_3D ( 'NONE', #20132, #10776, #12527 ) ;
#409 = CARTESIAN_POINT ( 'NONE',  ( 5.941205806953520074, 1.854262922671694143E-15, 15.14120580695351670 ) ) ;
#410 = DIRECTION ( 'NONE',  ( 0.000000000000000000, -1.000000000000000000, 0.000000000000000000 ) ) ;
#411 = PRODUCT_DEFINITION_FORMATION_WITH_SPECIFIED_SOURCE ( 'ANY', '', #7599, .NOT_KNOWN. ) ;
#412 = VECTOR ( 'NONE', #1213, 1000.000000000000000 ) ;
#413 = AXIS2_PLACEMENT_3D ( 'NONE', #8793, #15073, #19780 ) ;
#414 = ORIENTED_EDGE ( 'NONE', *, *, #903, .F. ) ;
#415 = CARTESIAN_POINT ( 'NONE',  ( 1.050000000000000044, 15.25000000000000000, 0.000000000000000000 ) ) ;
#416 = UNCERTAINTY_MEASURE_WITH_UNIT (LENGTH_MEASURE( 1.000000000000000082E-05 ), #13486, 'distance_accuracy_value', 'NONE');
#417 = VERTEX_POINT ( 'NONE', #9571 ) ;
#418 = ADVANCED_FACE ( 'NONE', ( #5059 ), #7835, .T. ) ;
#419 = CIRCLE ( 'NONE', #2387, 10.00000000000000888 ) ;
#420 = VECTOR ( 'NONE', #14227, 1000.000000000000000 ) ;
#421 = LINE ( 'NONE', #4872, #10566 ) ;
#422 = EDGE_LOOP ( 'NONE', ( #19212, #2987, #6932, #2338 ) ) ;
#423 = UNCERTAINTY_MEASURE_WITH_UNIT (LENGTH_MEASURE( 1.000000000000000082E-05 ), #18425, 'distance_accuracy_value', 'NONE');
#424 = CARTESIAN_POINT ( 'NONE',  ( -26.00000000000002842, 3.000000000000000000, -39.99999999999999289 ) ) ;
#425 = CARTESIAN_POINT ( 'NONE',  ( -39.99999999999997868, 3.000000000000000000, 26.00000000000000355 ) ) ;
#426 = UNCERTAINTY_MEASURE_WITH_UNIT (LENGTH_MEASURE( 1.000000000000000082E-05 ), #10471, 'distance_accuracy_value', 'NONE');
#427 = EDGE_LOOP ( 'NONE', ( #3778, #10463, #12858, #6820 ) ) ;
#428 = FACE_BOUND ( 'NONE', #9334, .T. ) ;
#429 = LINE ( 'NONE', #627, #7057 ) ;
#431 = EDGE_CURVE ( 'NONE', #10962, #10668, #11126, .T. ) ;
#430 = DIRECTION ( 'NONE',  ( -0.000000000000000000, -0.000000000000000000, 1.000000000000000000 ) ) ;
#432 = AXIS2_PLACEMENT_3D ( 'NONE', #1849, #20297, #3101 ) ;
#433 = VECTOR ( 'NONE', #12151, 1000.000000000000000 ) ;
#434 = FACE_OUTER_BOUND ( 'NONE', #2363, .T. ) ;
#435 = EDGE_CURVE ( 'NONE', #10328, #18338, #2769, .T. ) ;
#436 = ORIENTED_EDGE ( 'NONE', *, *, #16816, .T. ) ;
#437 =( NAMED_UNIT ( * ) PLANE_ANGLE_UNIT ( ) SI_UNIT ( $, .RADIAN. ) );
#438 = CARTESIAN_POINT ( 'NONE',  ( -81.18192946989275072, 140.4048636633015406, 499.8237260975782874 ) ) ;
#439 = PRESENTATION_LAYER_ASSIGNMENT (  '', '', ( #4065 ) ) ;
#440 = EDGE_CURVE ( 'NONE', #12019, #14963, #19152, .T. ) ;
#441 = DIRECTION ( 'NONE',  ( -1.000000000000000000, 0.000000000000000000, -0.000000000000000000 ) ) ;
#442 = EDGE_LOOP ( 'NONE', ( #17497, #7680, #6734, #2124 ) ) ;
#443 = EDGE_CURVE ( 'NONE', #39, #16841, #11331, .T. ) ;
#444 = PRESENTATION_LAYER_ASSIGNMENT (  '', '', ( #10004 ) ) ;
#445 = EDGE_LOOP ( 'NONE', ( #12077, #5510, #14819, #478 ) ) ;
#446 = EDGE_CURVE ( 'NONE', #19368, #19036, #134, .T. ) ;
#447 = EDGE_LOOP ( 'NONE', ( #14456, #1274 ) ) ;
#448 = CARTESIAN_POINT ( 'NONE',  ( -23.00000000000003197, 3.000000000000000000, 37.00000000000000711 ) ) ;
#449 = UNCERTAINTY_MEASURE_WITH_UNIT (LENGTH_MEASURE( 1.000000000000000082E-05 ), #13048, 'distance_accuracy_value', 'NONE');
#450 = PRESENTATION_LAYER_ASSIGNMENT (  '', '', ( #4747 ) ) ;
#451 = VECTOR ( 'NONE', #11887, 1000.000000000000000 ) ;
#452 = CARTESIAN_POINT ( 'NONE',  ( -1.274252908074454287E-14, 140.1563709946295262, 488.5655098179835818 ) ) ;
#453 = PLANE ( 'NONE',  #12031 ) ;
#454 = COLOUR_RGB ( '', 0.40784314, 0.44705882, 0.49803922) ;
#455 = LINE ( 'NONE', #13070, #20140 ) ;
#456 = PRESENTATION_STYLE_ASSIGNMENT (( #10433 ) ) ;
#457 = FACE_OUTER_BOUND ( 'NONE', #13528, .T. ) ;
#458 = VECTOR ( 'NONE', #18413, 1000.000000000000000 ) ;
#459 = ORIENTED_EDGE ( 'NONE', *, *, #4153, .F. ) ;
#460 = CARTESIAN_POINT ( 'NONE',  ( 486.8117674897343363, 214.2156642432025251, 250.0000000000000000 ) ) ;
#461 = FACE_BOUND ( 'NONE', #14046, .T. ) ;
#462 =( NAMED_UNIT ( * ) SI_UNIT ( $, .STERADIAN. ) SOLID_ANGLE_UNIT ( ) );
#463 =( NAMED_UNIT ( * ) PLANE_ANGLE_UNIT ( ) SI_UNIT ( $, .RADIAN. ) );
#464 = AXIS2_PLACEMENT_3D ( 'NONE', #7288, #2925, #17152 ) ;
#465 = CARTESIAN_POINT ( 'NONE',  ( 111.4893729001366012, 127.7247684487574588, 370.0000000000000000 ) ) ;
#466 = DIRECTION ( 'NONE',  ( 1.000000000000000000, 9.815121534730718631E-17, 0.000000000000000000 ) ) ;
#467 = EDGE_CURVE ( 'NONE', #1495, #8580, #14633, .T. ) ;
#468 = AXIS2_PLACEMENT_3D ( 'NONE', #18495, #1257, #15845 ) ;
#469 = VERTEX_POINT ( 'NONE', #9888 ) ;
#470 = VECTOR ( 'NONE', #9306, 1000.000000000000000 ) ;
#471 = AXIS2_PLACEMENT_3D ( 'NONE', #16641, #10625, #2793 ) ;
#472 = AXIS2_PLACEMENT_3D ( 'NONE', #19365, #14841, #16413 ) ;
#473 = EDGE_CURVE ( 'NONE', #9264, #2341, #13005, .T. ) ;
#474 = ORIENTED_EDGE ( 'NONE', *, *, #15207, .F. ) ;
#475 = B_SPLINE_CURVE_WITH_KNOTS ( 'NONE', 3,
 ( #13075, #4904, #12750, #13157, #19000, #3666, #17459, #5011, #3357, #3473, #9633, #15954, #6560, #11281, #9750, #2199, #18370, #657 ),
 .UNSPECIFIED., .F., .F.,
 ( 4, 2, 2, 2, 2, 2, 2, 2, 4 ),
 ( 0.004721323624227206743, 0.005310725018217476653, 0.005900126412207745696, 0.006489527806198015607, 0.007078929200188285517, 0.007668330594178554560, 0.008257731988168825338, 0.008847133382159092646, 0.009436534776149363424 ),
 .UNSPECIFIED. ) ;
#476 = EDGE_CURVE ( 'NONE', #17048, #8243, #2236, .T. ) ;
#477 = CIRCLE ( 'NONE', #18244, 3.300000000000000711 ) ;
#478 = ORIENTED_EDGE ( 'NONE', *, *, #4617, .T. ) ;
#479 = FILL_AREA_STYLE_COLOUR ( '', #3345 ) ;
#480 = DIRECTION ( 'NONE',  ( 0.000000000000000000, 0.000000000000000000, -1.000000000000000000 ) ) ;
#481 = AXIS2_PLACEMENT_3D ( 'NONE', #4264, #1133, #15084 ) ;
#482 = EDGE_LOOP ( 'NONE', ( #11298, #10691 ) ) ;
#483 = CARTESIAN_POINT ( 'NONE',  ( 10.00000000000000000, 306.0487089519832011, -75.00000000000380851 ) ) ;
#484 = DIRECTION ( 'NONE',  ( 0.000000000000000000, -1.000000000000000000, 0.000000000000000000 ) ) ;
#485 = ORIENTED_EDGE ( 'NONE', *, *, #11519, .T. ) ;
#486 = VECTOR ( 'NONE', #1460, 1000.000000000000000 ) ;
#487 = CARTESIAN_POINT ( 'NONE',  ( 0.6999999999999999556, 0.000000000000000000, 0.000000000000000000 ) ) ;
#488 = VECTOR ( 'NONE', #2515, 1000.000000000000000 ) ;
#489 = DIRECTION ( 'NONE',  ( 0.000000000000000000, 1.000000000000000000, 0.000000000000000000 ) ) ;
#490 = LINE ( 'NONE', #9659, #4444 ) ;
#491 = VECTOR ( 'NONE', #5469, 1000.000000000000000 ) ;
#492 = DIRECTION ( 'NONE',  ( 0.000000000000000000, 0.000000000000000000, 1.000000000000000000 ) ) ;
#493 = DIRECTION ( 'NONE',  ( -0.000000000000000000, -1.000000000000000000, -0.000000000000000000 ) ) ;
#494 = SHAPE_REPRESENTATION_RELATIONSHIP ( 'NONE' , 'NONE' ,  #10380, #14285 ) ;
#495 = DIRECTION ( 'NONE',  ( -0.000000000000000000, -1.000000000000000000, 0.000000000000000000 ) ) ;
#496 = CIRCLE ( 'NONE', #16324, 4.999999999999997335 ) ;
#497 = LINE ( 'NONE', #6115, #20364 ) ;
#498 = ORIENTED_EDGE ( 'NONE', *, *, #10417, .F. ) ;
#499 = DIRECTION ( 'NONE',  ( -0.000000000000000000, -1.000000000000000000, -1.632680918566406547E-16 ) ) ;
#500 = ORIENTED_EDGE ( 'NONE', *, *, #7079, .F. ) ;
#501 = COLOUR_RGB ( '', 0.72549020, 0.75294118, 0.79215686) ;
#502 = EDGE_CURVE ( 'NONE', #13110, #6513, #14954, .T. ) ;
#503 = VERTEX_POINT ( 'NONE', #13112 ) ;
#504 = VERTEX_POINT ( 'NONE', #11439 ) ;
#505 = AXIS2_PLACEMENT_3D ( 'NONE', #7155, #16926, #12173 ) ;
#506 = VERTEX_POINT ( 'NONE', #10189 ) ;
#507 = ORIENTED_EDGE ( 'NONE', *, *, #13292, .F. ) ;
#508 = DIRECTION ( 'NONE',  ( -0.9740972002433518906, -0.2261297071993489949, -2.769290221138109488E-17 ) ) ;
#509 = VECTOR ( 'NONE', #7959, 1000.000000000000000 ) ;
#510 = CARTESIAN_POINT ( 'NONE',  ( -21.85283368562565443, 317.7545334744432353, 485.1700099148404774 ) ) ;
#511 = CARTESIAN_POINT ( 'NONE',  ( 463.8334540492693350, 191.8198460455371333, 235.0057801310552463 ) ) ;
#512 = DIRECTION ( 'NONE',  ( -0.000000000000000000, 1.000000000000000000, 0.000000000000000000 ) ) ;
#513 = VECTOR ( 'NONE', #10974, 1000.000000000000000 ) ;
#514 = DIRECTION ( 'NONE',  ( 1.000000000000000000, -0.000000000000000000, 0.000000000000000000 ) ) ;
#515 = DIRECTION ( 'NONE',  ( -0.000000000000000000, -1.000000000000000000, -0.000000000000000000 ) ) ;
#516 = CARTESIAN_POINT ( 'NONE',  ( 2.999999999999998668, 60.19942049011861940, 9.013878188659973034 ) ) ;
#517 = CARTESIAN_POINT ( 'NONE',  ( 6.662140294759496685E-13, 139.7703989349477354, 490.5655098180907885 ) ) ;
#518 = CARTESIAN_POINT ( 'NONE',  ( 5.941205806953520074, -15.14120580695428764, -1.854262922671788806E-15 ) ) ;
#519 = PRESENTATION_STYLE_ASSIGNMENT (( #5068 ) ) ;
#520 = DIRECTION ( 'NONE',  ( 1.000000000000000000, 0.000000000000000000, 0.000000000000000000 ) ) ;
#521 =( NAMED_UNIT ( * ) SI_UNIT ( $, .STERADIAN. ) SOLID_ANGLE_UNIT ( ) );
#522 = DIRECTION ( 'NONE',  ( 1.450371633464475779E-15, -0.000000000000000000, 1.000000000000000000 ) ) ;
#523 = AXIS2_PLACEMENT_3D ( 'NONE', #2375, #835, #7149 ) ;
#524 = ADVANCED_BREP_SHAPE_REPRESENTATION ( '', ( #1644, #2741 ), #6708 ) ;
#525 = VECTOR ( 'NONE', #6100, 1000.000000000000000 ) ;
#526 = ORIENTED_EDGE ( 'NONE', *, *, #19912, .T. ) ;
#527 = EDGE_CURVE ( 'NONE', #5719, #9425, #9992, .T. ) ;
#528 = ORIENTED_EDGE ( 'NONE', *, *, #9807, .F. ) ;
#529 = CARTESIAN_POINT ( 'NONE',  ( 5.941205806953520074, 0.000000000000000000, 0.000000000000000000 ) ) ;
#530 = VERTEX_POINT ( 'NONE', #5261 ) ;
#531 = DIRECTION ( 'NONE',  ( -0.000000000000000000, -1.000000000000000000, -0.000000000000000000 ) ) ;
#532 = CARTESIAN_POINT ( 'NONE',  ( 3.000000000000000000, 41.00000000000000711, 6.000000000000000000 ) ) ;
#533 = ORIENTED_EDGE ( 'NONE', *, *, #18599, .F. ) ;
#534 = LINE ( 'NONE', #11248, #9722 ) ;
#535 = DIRECTION ( 'NONE',  ( -1.000000000000000000, -0.000000000000000000, -0.000000000000000000 ) ) ;
#536 = MECHANICAL_DESIGN_GEOMETRIC_PRESENTATION_REPRESENTATION (  '', ( #851 ), #3508 ) ;
#537 = CARTESIAN_POINT ( 'NONE',  ( -3.000000000000000000, 41.00000000000000711, 9.013878188659973034 ) ) ;
#538 = ADVANCED_FACE ( 'NONE', ( #5357, #3709 ), #13302, .T. ) ;
#539 = CIRCLE ( 'NONE', #19307, 0.9999999999999995559 ) ;
#540 = PRESENTATION_STYLE_ASSIGNMENT (( #9923 ) ) ;
#541 = CYLINDRICAL_SURFACE ( 'NONE', #732, 10.00000000000000888 ) ;
#542 = DIRECTION ( 'NONE',  ( 0.000000000000000000, 0.000000000000000000, -1.000000000000000000 ) ) ;
#543 = FACE_OUTER_BOUND ( 'NONE', #6094, .T. ) ;
#544 = ORIENTED_EDGE ( 'NONE', *, *, #15177, .T. ) ;
#545 = CYLINDRICAL_SURFACE ( 'NONE', #13470, 10.00000000000000888 ) ;
#546 = DIRECTION ( 'NONE',  ( 0.000000000000000000, 1.000000000000000000, 0.000000000000000000 ) ) ;
#547 = PLANE ( 'NONE',  #5073 ) ;
#548 = VERTEX_POINT ( 'NONE', #13204 ) ;
#549 = EDGE_CURVE ( 'NONE', #13739, #15829, #13960, .T. ) ;
#550 = ORIENTED_EDGE ( 'NONE', *, *, #7264, .F. ) ;
#551 = EDGE_LOOP ( 'NONE', ( #1473, #9474, #8309, #5277 ) ) ;
#552 = DIRECTION ( 'NONE',  ( 0.000000000000000000, 0.000000000000000000, 1.000000000000000000 ) ) ;
#553 = ADVANCED_FACE ( 'NONE', ( #16403 ), #14824, .F. ) ;
#554 = EDGE_LOOP ( 'NONE', ( #11061, #4996, #7000, #1431 ) ) ;
#555 = FILL_AREA_STYLE ('',( #14994 ) ) ;
#556 = CARTESIAN_POINT ( 'NONE',  ( 2.980268877975829511, 40.60428768742846728, 9.020512128682495856 ) ) ;
#557 = ORIENTED_EDGE ( 'NONE', *, *, #314, .F. ) ;
#558 = ADVANCED_FACE ( 'NONE', ( #11751 ), #3909, .T. ) ;
#559 = FILL_AREA_STYLE_COLOUR ( '', #17283 ) ;
#560 = ADVANCED_FACE ( 'NONE', ( #14938 ), #5654, .F. ) ;
#561 = EDGE_CURVE ( 'NONE', #9020, #14418, #12236, .T. ) ;
#562 = DIRECTION ( 'NONE',  ( 0.000000000000000000, 1.000000000000000000, 0.000000000000000000 ) ) ;
#563 = SURFACE_STYLE_FILL_AREA ( #8590 ) ;
#564 = CARTESIAN_POINT ( 'NONE',  ( 475.8334540492694487, 214.2156642432025251, 250.0000000000000000 ) ) ;
#565 = AXIS2_PLACEMENT_3D ( 'NONE', #517, #8653, #16502 ) ;
#566 = VERTEX_POINT ( 'NONE', #12354 ) ;
#567 = DIRECTION ( 'NONE',  ( 0.000000000000000000, 1.179611963664227814E-13, -1.000000000000000000 ) ) ;
#568 = EDGE_CURVE ( 'NONE', #9832, #5553, #10017, .T. ) ;
#569 = DIRECTION ( 'NONE',  ( 1.000000000000000000, 9.815121534730717399E-17, -0.000000000000000000 ) ) ;
#570 = CARTESIAN_POINT ( 'NONE',  ( 7.000000000000000000, -17.85000000000000142, -2.225795557450314789E-15 ) ) ;
#571 = DIRECTION ( 'NONE',  ( 1.000000000000000000, 0.000000000000000000, 0.000000000000000000 ) ) ;
#572 = CARTESIAN_POINT ( 'NONE',  ( -22.00000000000001776, 10.00000000000000000, 36.00000000000000711 ) ) ;
#573 = ORIENTED_EDGE ( 'NONE', *, *, #710, .T. ) ;
#574 = EDGE_CURVE ( 'NONE', #2140, #4998, #18228, .T. ) ;
#575 = ORIENTED_EDGE ( 'NONE', *, *, #4462, .T. ) ;
#576 = VECTOR ( 'NONE', #1762, 1000.000000000000000 ) ;
#577 = CIRCLE ( 'NONE', #20325, 3.300000000000011369 ) ;
#578 = ORIENTED_EDGE ( 'NONE', *, *, #8167, .T. ) ;
#579 = CARTESIAN_POINT ( 'NONE',  ( 458.8334540492693350, 191.8198460455371333, 91.76606011801541740 ) ) ;
#580 = LINE ( 'NONE', #19423, #7154 ) ;
#581 = ORIENTED_EDGE ( 'NONE', *, *, #2414, .F. ) ;
#582 = LINE ( 'NONE', #6893, #152 ) ;
#583 = DIRECTION ( 'NONE',  ( -0.000000000000000000, -1.000000000000000000, -0.000000000000000000 ) ) ;
#584 = VERTEX_POINT ( 'NONE', #2855 ) ;
#585 = EDGE_CURVE ( 'NONE', #12613, #10280, #7419, .T. ) ;
#586 = CARTESIAN_POINT ( 'NONE',  ( 37.00000000000000000, 68.00000000000000000, -23.00000000000000000 ) ) ;
#587 = CARTESIAN_POINT ( 'NONE',  ( 1.000000000001310507, 139.7703989349544997, 489.5655098179835818 ) ) ;
#588 = DIRECTION ( 'NONE',  ( 0.000000000000000000, 0.000000000000000000, -1.000000000000000000 ) ) ;
#589 = PLANE ( 'NONE',  #2792 ) ;
#590 = CARTESIAN_POINT ( 'NONE',  ( 178.4893729001365728, 123.1299228374914918, 220.6387154965113382 ) ) ;
#591 = CARTESIAN_POINT ( 'NONE',  ( 30.99999999999997513, 0.000000000000000000, 30.99999999999999645 ) ) ;
#592 = AXIS2_PLACEMENT_3D ( 'NONE', #9847, #2300, #6876 ) ;
#593 = VERTEX_POINT ( 'NONE', #981 ) ;
#594 = CARTESIAN_POINT ( 'NONE',  ( 463.8334540492693350, 214.2156642432025251, -87.31255586191144857 ) ) ;
#595 = ORIENTED_EDGE ( 'NONE', *, *, #3023, .T. ) ;
#596 = PRODUCT_DEFINITION_CONTEXT ( 'detailed design', #10521, 'design' ) ;
#597 = ORIENTED_EDGE ( 'NONE', *, *, #11865, .F. ) ;
#599 = ORIENTED_EDGE ( 'NONE', *, *, #17250, .T. ) ;
#598 = EDGE_CURVE ( 'NONE', #5524, #14262, #8850, .T. ) ;
#600 = EDGE_LOOP ( 'NONE', ( #18640, #5811 ) ) ;
#601 = CARTESIAN_POINT ( 'NONE',  ( 78.48937290013660117, 113.1299228374914208, 79.58252780074349175 ) ) ;
#602 = DIRECTION ( 'NONE',  ( 0.000000000000000000, 0.000000000000000000, -1.000000000000000000 ) ) ;
#603 = AXIS2_PLACEMENT_3D ( 'NONE', #20232, #17541, #4790 ) ;
#604 = FACE_OUTER_BOUND ( 'NONE', #19997, .T. ) ;
#605 = DIRECTION ( 'NONE',  ( 2.775557561562888827E-14, 0.000000000000000000, -1.000000000000000000 ) ) ;
#606 = CARTESIAN_POINT ( 'NONE',  ( 10.00000000000000000, 309.2289037985885898, -83.18019484660915452 ) ) ;
#607 = CYLINDRICAL_SURFACE ( 'NONE', #3748, 36.50000000000000000 ) ;
#608 = CARTESIAN_POINT ( 'NONE',  ( -31.00000000000000000, 11.00000000000000000, 30.99999999999999289 ) ) ;
#609 = LINE ( 'NONE', #12907, #9903 ) ;
#610 = PLANE ( 'NONE',  #16307 ) ;
#611 = FACE_OUTER_BOUND ( 'NONE', #3674, .T. ) ;
#612 = CIRCLE ( 'NONE', #8852, 0.9999999999999983347 ) ;
#613 = PRESENTATION_LAYER_ASSIGNMENT (  '', '', ( #2590 ) ) ;
#614 = ORIENTED_EDGE ( 'NONE', *, *, #18375, .F. ) ;
#615 = CARTESIAN_POINT ( 'NONE',  ( 153.4893729001366864, 123.1299228374914634, 29.36128450348865471 ) ) ;
#616 = UNCERTAINTY_MEASURE_WITH_UNIT (LENGTH_MEASURE( 1.000000000000000082E-05 ), #11139, 'distance_accuracy_value', 'NONE');
#617 = ORIENTED_EDGE ( 'NONE', *, *, #12282, .F. ) ;
#618 = ORIENTED_EDGE ( 'NONE', *, *, #12060, .T. ) ;
#619 = EDGE_LOOP ( 'NONE', ( #15258, #6627, #2026, #12309 ) ) ;
#620 = FACE_OUTER_BOUND ( 'NONE', #6910, .T. ) ;
#621 = UNCERTAINTY_MEASURE_WITH_UNIT (LENGTH_MEASURE( 1.000000000000000082E-05 ), #1117, 'distance_accuracy_value', 'NONE');
#622 = DIRECTION ( 'NONE',  ( -1.135258727068399668E-15, 0.000000000000000000, 1.000000000000000000 ) ) ;
#623 = DIRECTION ( 'NONE',  ( 1.000000000000000000, -0.000000000000000000, 0.000000000000000000 ) ) ;
#624 = VECTOR ( 'NONE', #19346, 1000.000000000000000 ) ;
#625 = VERTEX_POINT ( 'NONE', #4222 ) ;
#626 = CARTESIAN_POINT ( 'NONE',  ( 55.98937290013660117, 144.5787140289007198, 293.4524157190248275 ) ) ;
#627 = CARTESIAN_POINT ( 'NONE',  ( 111.4893729001366154, 77.72476844875745883, 250.0000000000000000 ) ) ;
#628 = ADVANCED_FACE ( 'NONE', ( #17001 ), #19748, .F. ) ;
#629 = CARTESIAN_POINT ( 'NONE',  ( 153.4893729001366580, 80.91625508013694912, 250.0000000000000000 ) ) ;
#630 = VECTOR ( 'NONE', #3391, 1000.000000000000000 ) ;
#631 = AXIS2_PLACEMENT_3D ( 'NONE', #7992, #9439, #17458 ) ;
#632 = DIRECTION ( 'NONE',  ( -0.000000000000000000, -1.000000000000000000, 0.000000000000000000 ) ) ;
#633 = FILL_AREA_STYLE_COLOUR ( '', #9221 ) ;
#634 = FACE_OUTER_BOUND ( 'NONE', #3655, .T. ) ;
#635 = ORIENTED_EDGE ( 'NONE', *, *, #2291, .F. ) ;
#636 = DIRECTION ( 'NONE',  ( 0.000000000000000000, 1.000000000000000000, 0.000000000000000000 ) ) ;
#637 =( LENGTH_UNIT ( ) NAMED_UNIT ( * ) SI_UNIT ( .MILLI., .METRE. ) );
#638 = CARTESIAN_POINT ( 'NONE',  ( 111.4893729001366012, 127.7247684487574588, 368.0000000000000000 ) ) ;
#639 = COLOUR_RGB ( '', 0.66274510, 0.83137255, 0.94901961) ;
#640 = PRESENTATION_LAYER_ASSIGNMENT (  '', '', ( #5921 ) ) ;
#641 = CIRCLE ( 'NONE', #1256, 4.999999999999997335 ) ;
#642 = EDGE_CURVE ( 'NONE', #11944, #19482, #11992, .T. ) ;
#643 = ORIENTED_EDGE ( 'NONE', *, *, #13866, .T. ) ;
#644 = FACE_OUTER_BOUND ( 'NONE', #17782, .T. ) ;
#645 = VERTEX_POINT ( 'NONE', #16792 ) ;
#646 = CARTESIAN_POINT ( 'NONE',  ( 463.8334540492693350, 191.8198460455371333, 24.99421986894476078 ) ) ;
#647 = CARTESIAN_POINT ( 'NONE',  ( 0.3928280596732524055, 38.01925660030116205, 9.493865254640489582 ) ) ;
#648 = ORIENTED_EDGE ( 'NONE', *, *, #12936, .T. ) ;
#649 = CARTESIAN_POINT ( 'NONE',  ( -1.000000000000004885, 146.1184945051221860, 507.7561228916242158 ) ) ;
#650 = CARTESIAN_POINT ( 'NONE',  ( 7.000000000000000000, 0.000000000000000000, 0.000000000000000000 ) ) ;
#651 = CARTESIAN_POINT ( 'NONE',  ( 111.4893729001366154, 49.66333933884488516, 252.0000000000000000 ) ) ;
#652 = CIRCLE ( 'NONE', #15493, 9.000000000000007105 ) ;
#653 = AXIS2_PLACEMENT_3D ( 'NONE', #4126, #7308, #10403 ) ;
#654 = FILL_AREA_STYLE ('',( #11708 ) ) ;
#655 = EDGE_CURVE ( 'NONE', #3196, #7067, #16936, .T. ) ;
#656 = VECTOR ( 'NONE', #19292, 1000.000000000000000 ) ;
#657 = CARTESIAN_POINT ( 'NONE',  ( -3.000000000000000000, 41.00000000000000711, 9.013878188659973034 ) ) ;
#658 = VERTEX_POINT ( 'NONE', #16896 ) ;
#659 = DIRECTION ( 'NONE',  ( -0.000000000000000000, -1.000000000000000000, 0.000000000000000000 ) ) ;
#660 = DIRECTION ( 'NONE',  ( 0.000000000000000000, 0.000000000000000000, 1.000000000000000000 ) ) ;
#661 = CARTESIAN_POINT ( 'NONE',  ( 0.000000000000000000, 216.7545334744432921, 155.1946179577816167 ) ) ;
#662 = EDGE_CURVE ( 'NONE', #3606, #3463, #9152, .T. ) ;
#663 = PLANE ( 'NONE',  #3342 ) ;
#664 = VERTEX_POINT ( 'NONE', #4311 ) ;
#665 = ORIENTED_EDGE ( 'NONE', *, *, #16444, .F. ) ;
#666 = VERTEX_POINT ( 'NONE', #19853 ) ;
#667 = EDGE_CURVE ( 'NONE', #1728, #12429, #6413, .T. ) ;
#668 = VECTOR ( 'NONE', #2486, 1000.000000000000114 ) ;
#669 = EDGE_LOOP ( 'NONE', ( #5288, #16345, #8845, #9918 ) ) ;
#670 = ORIENTED_EDGE ( 'NONE', *, *, #7353, .F. ) ;
#671 = DIRECTION ( 'NONE',  ( 1.000000000000000000, 9.815121534730717399E-17, 0.000000000000000000 ) ) ;
#672 = EDGE_CURVE ( 'NONE', #5981, #6883, #1099, .T. ) ;
#673 = LINE ( 'NONE', #19332, #17014 ) ;
#674 = ORIENTED_EDGE ( 'NONE', *, *, #1549, .F. ) ;
#675 = DIRECTION ( 'NONE',  ( 1.000000000000000000, 0.000000000000000000, 0.000000000000000000 ) ) ;
#676 = ORIENTED_EDGE ( 'NONE', *, *, #12915, .T. ) ;
#677 = CARTESIAN_POINT ( 'NONE',  ( -26.00000000000002132, 0.000000000000000000, 40.00000000000000711 ) ) ;
#678 = LINE ( 'NONE', #17896, #2364 ) ;
#679 = CARTESIAN_POINT ( 'NONE',  ( 0.3266166635162791043, 138.8954520623098006, 489.3238097202654444 ) ) ;
#680 = EDGE_CURVE ( 'NONE', #13953, #18077, #20051, .T. ) ;
#681 = LINE ( 'NONE', #8232, #5072 ) ;
#682 = DIRECTION ( 'NONE',  ( 0.000000000000000000, 1.000000000000000000, 0.000000000000000000 ) ) ;
#683 = CARTESIAN_POINT ( 'NONE',  ( 30.99999999999995737, 3.000000000000000000, 31.00000000000000000 ) ) ;
#684 = VECTOR ( 'NONE', #4855, 1000.000000000000000 ) ;
#685 = FACE_OUTER_BOUND ( 'NONE', #7571, .T. ) ;
#686 = UNCERTAINTY_MEASURE_WITH_UNIT (LENGTH_MEASURE( 1.000000000000000082E-05 ), #915, 'distance_accuracy_value', 'NONE');
#687 = DIRECTION ( 'NONE',  ( 0.000000000000000000, 1.000000000000000000, 0.000000000000000000 ) ) ;
#688 = VERTEX_POINT ( 'NONE', #2759 ) ;
#689 = EDGE_CURVE ( 'NONE', #17495, #15985, #20159, .T. ) ;
#690 = ORIENTED_EDGE ( 'NONE', *, *, #19539, .T. ) ;
#691 = EDGE_CURVE ( 'NONE', #17286, #13581, #15353, .T. ) ;
#692 = ORIENTED_EDGE ( 'NONE', *, *, #15699, .T. ) ;
#693 = VERTEX_POINT ( 'NONE', #1085 ) ;
#694 = ORIENTED_EDGE ( 'NONE', *, *, #2943, .T. ) ;
#695 = FILL_AREA_STYLE ('',( #7211 ) ) ;
#696 = CIRCLE ( 'NONE', #11915, 4.999999999999997335 ) ;
#697 = DIRECTION ( 'NONE',  ( -1.000000000000000000, 0.000000000000000000, -0.000000000000000000 ) ) ;
#698 = CARTESIAN_POINT ( 'NONE',  ( -31.00000000000006750, 3.000000000000000000, 26.00000000000000355 ) ) ;
#699 = CARTESIAN_POINT ( 'NONE',  ( 1.224646799147351235E-16, 65.20000000000000284, -0.9999999999999988898 ) ) ;
#700 = AXIS2_PLACEMENT_3D ( 'NONE', #2118, #9651, #2004 ) ;
#701 = CARTESIAN_POINT ( 'NONE',  ( 423.8334540492694487, 191.8198460455371333, 225.0057801310552463 ) ) ;
#702 = CARTESIAN_POINT ( 'NONE',  ( 4.899999999999999467, 0.000000000000000000, 0.000000000000000000 ) ) ;
#703 = LINE ( 'NONE', #19653, #11446 ) ;
#704 = CARTESIAN_POINT ( 'NONE',  ( -80.02433601516246142, 140.0032791352475101, 488.8200091561060958 ) ) ;
#705 = ADVANCED_FACE ( 'NONE', ( #1184 ), #8050, .T. ) ;
#706 = DIRECTION ( 'NONE',  ( 0.000000000000000000, 1.000000000000000000, 0.000000000000000000 ) ) ;
#707 = CARTESIAN_POINT ( 'NONE',  ( 143.0892156028631348, 80.91625508013694912, 245.0000000000000000 ) ) ;
#708 = AXIS2_PLACEMENT_3D ( 'NONE', #14152, #7971, #18986 ) ;
#709 = PRESENTATION_LAYER_ASSIGNMENT (  '', '', ( #9594 ) ) ;
#710 = EDGE_CURVE ( 'NONE', #1294, #4484, #4521, .T. ) ;
#711 = ORIENTED_EDGE ( 'NONE', *, *, #816, .F. ) ;
#712 = ORIENTED_EDGE ( 'NONE', *, *, #19124, .F. ) ;
#713 = AXIS2_PLACEMENT_3D ( 'NONE', #15673, #10911, #4930 ) ;
#714 = FACE_OUTER_BOUND ( 'NONE', #5598, .T. ) ;
#715 = VERTEX_POINT ( 'NONE', #6181 ) ;
#716 = VERTEX_POINT ( 'NONE', #12767 ) ;
#717 = FILL_AREA_STYLE ('',( #10208 ) ) ;
#718 = DIRECTION ( 'NONE',  ( 0.000000000000000000, 1.000000000000000000, 0.000000000000000000 ) ) ;
#719 = VECTOR ( 'NONE', #11315, 1000.000000000000000 ) ;
#720 = VECTOR ( 'NONE', #2438, 1000.000000000000000 ) ;
#721 = PLANE ( 'NONE',  #20067 ) ;
#722 = CARTESIAN_POINT ( 'NONE',  ( 98.48937290013662960, 1.571051285554951424E-14, -97.94896630388704750 ) ) ;
#723 = DIRECTION ( 'NONE',  ( -0.000000000000000000, -1.000000000000000000, -0.000000000000000000 ) ) ;
#724 = CARTESIAN_POINT ( 'NONE',  ( 153.4893729001366864, 113.1299228374914634, 79.58252780074349175 ) ) ;
#725 = MECHANICAL_DESIGN_GEOMETRIC_PRESENTATION_REPRESENTATION (  '', ( #15898 ), #10286 ) ;
#726 =( NAMED_UNIT ( * ) PLANE_ANGLE_UNIT ( ) SI_UNIT ( $, .RADIAN. ) );
#727 = CARTESIAN_POINT ( 'NONE',  ( 3.000000000000000000, 6.000000000000000000, 3.000000000000000000 ) ) ;
#728 = CARTESIAN_POINT ( 'NONE',  ( -34.99999999999999289, 8.000000000000000000, -35.00000000000000711 ) ) ;
#729 = VECTOR ( 'NONE', #9175, 1000.000000000000000 ) ;
#730 = EDGE_LOOP ( 'NONE', ( #10944, #17357 ) ) ;
#731 = CARTESIAN_POINT ( 'NONE',  ( -40.00000000000000711, 10.00000000000000000, 26.00000000000000000 ) ) ;
#732 = AXIS2_PLACEMENT_3D ( 'NONE', #13342, #19587, #11368 ) ;
#733 = CARTESIAN_POINT ( 'NONE',  ( 34.99999999999997868, 8.000000000000000000, -40.00000000000000711 ) ) ;
#734 = COLOUR_RGB ( '', 0.66274510, 0.83137255, 0.94901961) ;
#735 = AXIS2_PLACEMENT_3D ( 'NONE', #5851, #16780, #4505 ) ;
#736 = ADVANCED_FACE ( 'NONE', ( #6582 ), #17594, .F. ) ;
#737 = PRESENTATION_LAYER_ASSIGNMENT (  '', '', ( #9634 ) ) ;
#738 = VERTEX_POINT ( 'NONE', #11105 ) ;
#739 = EDGE_LOOP ( 'NONE', ( #2675, #7666, #18295, #18706 ) ) ;
#740 = EDGE_LOOP ( 'NONE', ( #19768, #8935, #9607, #17560 ) ) ;
#741 = CARTESIAN_POINT ( 'NONE',  ( 35.00000000000000711, 11.00000000000000000, -35.00000000000000711 ) ) ;
#742 = CARTESIAN_POINT ( 'NONE',  ( -20.00000000000003197, 3.000000000000000000, 40.00000000000000711 ) ) ;
#743 = ORIENTED_EDGE ( 'NONE', *, *, #527, .F. ) ;
#744 = CARTESIAN_POINT ( 'NONE',  ( 22.99999999999998224, 10.00000000000000000, -36.99999999999999289 ) ) ;
#745 =( NAMED_UNIT ( * ) SI_UNIT ( $, .STERADIAN. ) SOLID_ANGLE_UNIT ( ) );
#746 = PLANE ( 'NONE',  #16845 ) ;
#747 =( GEOMETRIC_REPRESENTATION_CONTEXT ( 3 ) GLOBAL_UNCERTAINTY_ASSIGNED_CONTEXT ( ( #13224 ) ) GLOBAL_UNIT_ASSIGNED_CONTEXT ( ( #19279, #14431, #19158 ) ) REPRESENTATION_CONTEXT ( 'NONE', 'WORKASPACE' ) );
#748 = STYLED_ITEM ( 'NONE', ( #406 ), #18434 ) ;
#749 = UNCERTAINTY_MEASURE_WITH_UNIT (LENGTH_MEASURE( 1.000000000000000082E-05 ), #9296, 'distance_accuracy_value', 'NONE');
#750 = CARTESIAN_POINT ( 'NONE',  ( 463.8334540492693350, 214.2156642432025251, 250.0000000000000000 ) ) ;
#751 = DIRECTION ( 'NONE',  ( 1.000000000000000000, 0.000000000000000000, 0.000000000000000000 ) ) ;
#752 = ORIENTED_EDGE ( 'NONE', *, *, #1611, .F. ) ;
#753 = FACE_OUTER_BOUND ( 'NONE', #19102, .T. ) ;
#754 = CARTESIAN_POINT ( 'NONE',  ( 55.48937290013660117, 127.7247684487574588, 370.0000000000000000 ) ) ;
#755 = DIRECTION ( 'NONE',  ( 0.000000000000000000, -1.632680918566406547E-16, 1.000000000000000000 ) ) ;
#756 = FILL_AREA_STYLE_COLOUR ( '', #7055 ) ;
#757 = EDGE_CURVE ( 'NONE', #10287, #3606, #812, .T. ) ;
#758 = VERTEX_POINT ( 'NONE', #12662 ) ;
#759 = VECTOR ( 'NONE', #16819, 1000.000000000000000 ) ;
#760 = DIRECTION ( 'NONE',  ( 1.000000000000000000, 0.000000000000000000, 0.000000000000000000 ) ) ;
#761 = ORIENTED_EDGE ( 'NONE', *, *, #14778, .T. ) ;
#762 = EDGE_LOOP ( 'NONE', ( #10042, #10538 ) ) ;
#763 = ORIENTED_EDGE ( 'NONE', *, *, #17421, .F. ) ;
#764 = AXIS2_PLACEMENT_3D ( 'NONE', #7394, #5745, #11928 ) ;
#765 = AXIS2_PLACEMENT_3D ( 'NONE', #12536, #17276, #3164 ) ;
#766 = CIRCLE ( 'NONE', #5404, 3.883636366625808911 ) ;
#767 = EDGE_CURVE ( 'NONE', #15180, #6572, #6476, .T. ) ;
#768 = ORIENTED_EDGE ( 'NONE', *, *, #15496, .T. ) ;
#769 = ORIENTED_EDGE ( 'NONE', *, *, #17561, .T. ) ;
#770 = LINE ( 'NONE', #11506, #19618 ) ;
#771 = EDGE_LOOP ( 'NONE', ( #8188, #13263, #7189, #7082 ) ) ;
#772 = FACE_OUTER_BOUND ( 'NONE', #3860, .T. ) ;
#773 = VECTOR ( 'NONE', #17341, 1000.000000000000000 ) ;
#774 = VECTOR ( 'NONE', #14732, 1000.000000000000000 ) ;
#775 = PRODUCT_RELATED_PRODUCT_CATEGORY ( 'part', '', ( #10900 ) ) ;
#776 = SURFACE_STYLE_FILL_AREA ( #13478 ) ;
#777 = LINE ( 'NONE', #17700, #16236 ) ;
#778 = CARTESIAN_POINT ( 'NONE',  ( 0.05191788718346542625, 139.0018976549732201, 488.9266887137286517 ) ) ;
#779 = DIRECTION ( 'NONE',  ( -1.000000000000000000, -0.000000000000000000, -0.000000000000000000 ) ) ;
#780 = LINE ( 'NONE', #3692, #4544 ) ;
#781 = EDGE_CURVE ( 'NONE', #8469, #13165, #477, .T. ) ;
#782 =( GEOMETRIC_REPRESENTATION_CONTEXT ( 3 ) GLOBAL_UNCERTAINTY_ASSIGNED_CONTEXT ( ( #5189 ) ) GLOBAL_UNIT_ASSIGNED_CONTEXT ( ( #19529, #3895, #15120 ) ) REPRESENTATION_CONTEXT ( 'NONE', 'WORKASPACE' ) );
#783 = VECTOR ( 'NONE', #8885, 1000.000000000000000 ) ;
#785 = VECTOR ( 'NONE', #5066, 1000.000000000000000 ) ;
#784 = FACE_OUTER_BOUND ( 'NONE', #12554, .T. ) ;
#786 = DIRECTION ( 'NONE',  ( 0.000000000000000000, 0.000000000000000000, 1.000000000000000000 ) ) ;
#787 = MECHANICAL_DESIGN_GEOMETRIC_PRESENTATION_REPRESENTATION (  '', ( #13630 ), #7704 ) ;
#788 = SURFACE_STYLE_FILL_AREA ( #11933 ) ;
#789 = CARTESIAN_POINT ( 'NONE',  ( 10.00000000000000000, 372.8685141053778693, -86.48019484660871115 ) ) ;
#790 = LINE ( 'NONE', #6908, #624 ) ;
#791 = EDGE_CURVE ( 'NONE', #8200, #19572, #14315, .T. ) ;
#792 = VERTEX_POINT ( 'NONE', #6275 ) ;
#793 = VECTOR ( 'NONE', #13436, 1000.000000000000000 ) ;
#794 = VECTOR ( 'NONE', #14802, 1000.000000000000000 ) ;
#795 = ORIENTED_EDGE ( 'NONE', *, *, #5988, .T. ) ;
#796 = PRODUCT_DEFINITION_CONTEXT ( 'detailed design', #9467, 'design' ) ;
#797 = ORIENTED_EDGE ( 'NONE', *, *, #3489, .F. ) ;
#798 = EDGE_CURVE ( 'NONE', #15238, #5834, #12871, .T. ) ;
#799 = ORIENTED_EDGE ( 'NONE', *, *, #19683, .T. ) ;
#800 = MECHANICAL_DESIGN_GEOMETRIC_PRESENTATION_REPRESENTATION (  '', ( #14301 ), #15294 ) ;
#801 = PRESENTATION_STYLE_ASSIGNMENT (( #19643 ) ) ;
#802 = FILL_AREA_STYLE_COLOUR ( '', #12303 ) ;
#803 = CARTESIAN_POINT ( 'NONE',  ( -31.00000000000003197, 19.00000000000000000, -26.00000000000000355 ) ) ;
#804 =( NAMED_UNIT ( * ) PLANE_ANGLE_UNIT ( ) SI_UNIT ( $, .RADIAN. ) );
#805 = EDGE_CURVE ( 'NONE', #8633, #7485, #11007, .T. ) ;
#806 = CARTESIAN_POINT ( 'NONE',  ( 423.8334540492694487, 191.8198460455371333, 225.0057801310552463 ) ) ;
#807 = CARTESIAN_POINT ( 'NONE',  ( 4.549999999999999822, 0.000000000000000000, 0.000000000000000000 ) ) ;
#808 = ADVANCED_FACE ( 'NONE', ( #15862 ), #15983, .T. ) ;
#809 = PRESENTATION_LAYER_ASSIGNMENT (  '', '', ( #14649 ) ) ;
#810 = CARTESIAN_POINT ( 'NONE',  ( -40.00000000000000000, 19.00000000000000000, -26.00000000000000355 ) ) ;
#811 = SURFACE_STYLE_USAGE ( .BOTH. , #14948 ) ;
#812 = CIRCLE ( 'NONE', #17588, 3.000000000000002665 ) ;
#813 = LINE ( 'NONE', #2155, #3205 ) ;
#814 = DIRECTION ( 'NONE',  ( 1.000000000000000000, 5.889072920838430686E-16, -0.000000000000000000 ) ) ;
#815 = PRESENTATION_STYLE_ASSIGNMENT (( #13601 ) ) ;
#816 = EDGE_CURVE ( 'NONE', #15238, #4974, #1821, .T. ) ;
#817 = CARTESIAN_POINT ( 'NONE',  ( 0.000000000000000000, 141.3905724437643698, 484.7051316060566819 ) ) ;
#818 = PRESENTATION_STYLE_ASSIGNMENT (( #9905 ) ) ;
#819 = EDGE_CURVE ( 'NONE', #16767, #4371, #5034, .T. ) ;
#820 = VECTOR ( 'NONE', #10129, 1000.000000000000000 ) ;
#821 = LINE ( 'NONE', #10201, #470 ) ;
#822 =( GEOMETRIC_REPRESENTATION_CONTEXT ( 3 ) GLOBAL_UNCERTAINTY_ASSIGNED_CONTEXT ( ( #8467 ) ) GLOBAL_UNIT_ASSIGNED_CONTEXT ( ( #15028, #2641, #15338 ) ) REPRESENTATION_CONTEXT ( 'NONE', 'WORKASPACE' ) );
#823 = STYLED_ITEM ( 'NONE', ( #3664 ), #14509 ) ;
#824 = ORIENTED_EDGE ( 'NONE', *, *, #16378, .T. ) ;
#825 = VERTEX_POINT ( 'NONE', #15764 ) ;
#826 = PRESENTATION_LAYER_ASSIGNMENT (  '', '', ( #5450 ) ) ;
#827 = ADVANCED_FACE ( 'NONE', ( #3490 ), #1593, .F. ) ;
#828 = FILL_AREA_STYLE ('',( #10423 ) ) ;
#829 = ORIENTED_EDGE ( 'NONE', *, *, #689, .F. ) ;
#830 = ORIENTED_EDGE ( 'NONE', *, *, #15569, .T. ) ;
#831 = AXIS2_PLACEMENT_3D ( 'NONE', #8730, #9188, #6122 ) ;
#832 = DIRECTION ( 'NONE',  ( 0.000000000000000000, 0.000000000000000000, 1.000000000000000000 ) ) ;
#833 = UNCERTAINTY_MEASURE_WITH_UNIT (LENGTH_MEASURE( 1.000000000000000082E-05 ), #11594, 'distance_accuracy_value', 'NONE');
#834 = ORIENTED_EDGE ( 'NONE', *, *, #8890, .F. ) ;
#835 = DIRECTION ( 'NONE',  ( -1.322948291343119651E-12, 0.000000000000000000, 1.000000000000000000 ) ) ;
#836 = CARTESIAN_POINT ( 'NONE',  ( 53.48937290013658696, 113.1299228374914065, 79.58252780074349175 ) ) ;
#837 = DIRECTION ( 'NONE',  ( 0.000000000000000000, 1.000000000000000000, 0.000000000000000000 ) ) ;
#838 = CARTESIAN_POINT ( 'NONE',  ( 498.8334540492693918, 191.8198460455371333, 71.76606011801538898 ) ) ;
#839 = EDGE_CURVE ( 'NONE', #19516, #19767, #11418, .T. ) ;
#840 = PLANE ( 'NONE',  #1106 ) ;
#841 = COLOUR_RGB ( '', 0.72549020, 0.75294118, 0.79215686) ;
#842 = CARTESIAN_POINT ( 'NONE',  ( -36.00000000000000711, 8.000000000000000000, -22.00000000000000355 ) ) ;
#843 = EDGE_CURVE ( 'NONE', #18080, #16176, #8398, .T. ) ;
#844 = ORIENTED_EDGE ( 'NONE', *, *, #781, .T. ) ;
#845 = CARTESIAN_POINT ( 'NONE',  ( -39.99999999999997868, 0.000000000000000000, 26.00000000000000355 ) ) ;
#846 = DIRECTION ( 'NONE',  ( 1.000000000000000000, 0.000000000000000000, 0.000000000000000000 ) ) ;
#847 = EDGE_CURVE ( 'NONE', #1341, #4687, #19625, .T. ) ;
#848 = AXIS2_PLACEMENT_3D ( 'NONE', #19398, #6769, #17968 ) ;
#849 = ORIENTED_EDGE ( 'NONE', *, *, #19801, .F. ) ;
#850 = ORIENTED_EDGE ( 'NONE', *, *, #6624, .T. ) ;
#851 = STYLED_ITEM ( 'NONE', ( #18019 ), #2851 ) ;
#852 = ORIENTED_EDGE ( 'NONE', *, *, #8790, .F. ) ;
#853 = PLANE ( 'NONE',  #17110 ) ;
#854 = UNCERTAINTY_MEASURE_WITH_UNIT (LENGTH_MEASURE( 1.000000000000000082E-05 ), #13674, 'distance_accuracy_value', 'NONE');
#855 = ORIENTED_EDGE ( 'NONE', *, *, #1066, .F. ) ;
#856 = DIRECTION ( 'NONE',  ( 3.854941057726246479E-16, 0.000000000000000000, -1.000000000000000000 ) ) ;
#857 = CYLINDRICAL_SURFACE ( 'NONE', #9362, 10.00000000000000888 ) ;
#858 = LINE ( 'NONE', #8307, #16439 ) ;
#859 = EDGE_CURVE ( 'NONE', #9269, #17763, #14910, .T. ) ;
#860 = DIRECTION ( 'NONE',  ( -0.000000000000000000, 1.000000000000000000, -0.000000000000000000 ) ) ;
#861 = ORIENTED_EDGE ( 'NONE', *, *, #4153, .T. ) ;
#862 = FILL_AREA_STYLE_COLOUR ( '', #8842 ) ;
#863 = CARTESIAN_POINT ( 'NONE',  ( -31.00000000000001776, 10.00000000000000000, 31.00000000000000000 ) ) ;
#864 =( LENGTH_UNIT ( ) NAMED_UNIT ( * ) SI_UNIT ( .MILLI., .METRE. ) );
#865 = VERTEX_POINT ( 'NONE', #16081 ) ;
#866 = CIRCLE ( 'NONE', #6480, 9.000000000000007105 ) ;
#867 = VERTEX_POINT ( 'NONE', #483 ) ;
#868 = ORIENTED_EDGE ( 'NONE', *, *, #3484, .T. ) ;
#869 = EDGE_LOOP ( 'NONE', ( #267, #17312, #12229, #6451 ) ) ;
#870 = PLANE ( 'NONE',  #13691 ) ;
#871 = CARTESIAN_POINT ( 'NONE',  ( 23.00000000000000711, 68.00000000000000000, -31.00000000000002487 ) ) ;
#872 = ORIENTED_EDGE ( 'NONE', *, *, #10810, .F. ) ;
#873 = PLANE ( 'NONE',  #2277 ) ;
#874 = DIRECTION ( 'NONE',  ( 0.000000000000000000, 0.000000000000000000, -1.000000000000000000 ) ) ;
#875 = CARTESIAN_POINT ( 'NONE',  ( 1.000000000001388889, 138.8314847490560169, 489.5655098179835818 ) ) ;
#876 = EDGE_CURVE ( 'NONE', #19179, #305, #7095, .T. ) ;
#877 = CARTESIAN_POINT ( 'NONE',  ( 40.00000000000000711, 8.000000000000000000, -34.99999999999997868 ) ) ;
#878 = DIRECTION ( 'NONE',  ( 8.659560562354968603E-17, 0.7071067811865445751, -0.7071067811865504593 ) ) ;
#879 = LINE ( 'NONE', #5540, #10619 ) ;
#880 = CARTESIAN_POINT ( 'NONE',  ( 503.8334540492693918, 0.000000000000000000, 250.0000000000000000 ) ) ;
#881 = PLANE ( 'NONE',  #12337 ) ;
#882 = DIRECTION ( 'NONE',  ( -9.815121534730717399E-17, 1.000000000000000000, -2.352167425053297897E-16 ) ) ;
#883 = PLANE ( 'NONE',  #10834 ) ;
#884 = PLANE ( 'NONE',  #5653 ) ;
#885 = CARTESIAN_POINT ( 'NONE',  ( 53.48937290013659407, 129.7247684487574304, 252.0000000000000000 ) ) ;
#886 = VERTEX_POINT ( 'NONE', #9864 ) ;
#887 = VECTOR ( 'NONE', #4863, 1000.000000000000000 ) ;
#888 = ORIENTED_EDGE ( 'NONE', *, *, #3213, .T. ) ;
#889 = VERTEX_POINT ( 'NONE', #8327 ) ;
#890 = EDGE_CURVE ( 'NONE', #13927, #19179, #16314, .T. ) ;
#891 = DIRECTION ( 'NONE',  ( -1.132388935707081510E-15, 0.000000000000000000, 1.000000000000000000 ) ) ;
#892 = CARTESIAN_POINT ( 'NONE',  ( 0.000000000000000000, 309.2289037985890445, -146.8198051533984199 ) ) ;
#893 = FILL_AREA_STYLE ('',( #20161 ) ) ;
#894 = VECTOR ( 'NONE', #17242, 1000.000000000000000 ) ;
#895 = FACE_OUTER_BOUND ( 'NONE', #16379, .T. ) ;
#896 = CARTESIAN_POINT ( 'NONE',  ( -79.99999999999995737, 142.0976792249508946, 485.4122383872432351 ) ) ;
#897 = CARTESIAN_POINT ( 'NONE',  ( -40.00000000000000711, 8.000000000000000000, -26.00000000000000000 ) ) ;
#898 = AXIS2_PLACEMENT_3D ( 'NONE', #20061, #4230, #15564 ) ;
#899 =( NAMED_UNIT ( * ) PLANE_ANGLE_UNIT ( ) SI_UNIT ( $, .RADIAN. ) );
#900 = DIRECTION ( 'NONE',  ( -1.000000000000000000, 0.000000000000000000, 0.000000000000000000 ) ) ;
#901 = DIRECTION ( 'NONE',  ( 1.000000000000000000, 0.000000000000000000, 0.000000000000000000 ) ) ;
#902 = DIRECTION ( 'NONE',  ( -0.000000000000000000, -0.000000000000000000, 1.000000000000000000 ) ) ;
#903 = EDGE_CURVE ( 'NONE', #6513, #13719, #369, .T. ) ;
#904 = DIRECTION ( 'NONE',  ( -1.000000000000000000, 0.000000000000000000, 0.000000000000000000 ) ) ;
#905 = EDGE_CURVE ( 'NONE', #14745, #1444, #5237, .T. ) ;
#906 = ORIENTED_EDGE ( 'NONE', *, *, #9151, .T. ) ;
#907 = ORIENTED_EDGE ( 'NONE', *, *, #8396, .F. ) ;
#908 = ORIENTED_EDGE ( 'NONE', *, *, #7465, .T. ) ;
#909 = ORIENTED_EDGE ( 'NONE', *, *, #4428, .F. ) ;
#910 = EDGE_CURVE ( 'NONE', #10871, #16657, #3115, .T. ) ;
#911 = EDGE_LOOP ( 'NONE', ( #11381, #8892, #12685, #4970 ) ) ;
#912 = FILL_AREA_STYLE_COLOUR ( '', #15271 ) ;
#913 = DIRECTION ( 'NONE',  ( -1.000000000000000000, -0.000000000000000000, 1.156482317317883755E-15 ) ) ;
#914 = EDGE_CURVE ( 'NONE', #10510, #4609, #14497, .T. ) ;
#915 =( LENGTH_UNIT ( ) NAMED_UNIT ( * ) SI_UNIT ( .MILLI., .METRE. ) );
#916 = CARTESIAN_POINT ( 'NONE',  ( -36.00000000000000000, 4.408728476930470856E-15, 0.000000000000000000 ) ) ;
#917 = LINE ( 'NONE', #7452, #14906 ) ;
#918 = CARTESIAN_POINT ( 'NONE',  ( -58.16843972078500258, 319.7545334744432353, 485.1700099148404206 ) ) ;
#919 = SURFACE_STYLE_USAGE ( .BOTH. , #15072 ) ;
#920 = CARTESIAN_POINT ( 'NONE',  ( -33.99999999999997158, 0.000000000000000000, -22.99999999999999645 ) ) ;
#921 = CARTESIAN_POINT ( 'NONE',  ( -80.73513083854561501, 138.7723821183164148, 490.5025619529872642 ) ) ;
#922 = LINE ( 'NONE', #11883, #18596 ) ;
#923 = EDGE_CURVE ( 'NONE', #1858, #17019, #582, .T. ) ;
#924 = CIRCLE ( 'NONE', #12471, 3.300000000000004263 ) ;
#925 = ORIENTED_EDGE ( 'NONE', *, *, #1375, .F. ) ;
#926 = DIRECTION ( 'NONE',  ( 0.000000000000000000, 1.000000000000000000, -0.000000000000000000 ) ) ;
#927 = FACE_BOUND ( 'NONE', #7352, .T. ) ;
#928 = ADVANCED_FACE ( 'NONE', ( #772 ), #17891, .T. ) ;
#929 = ORIENTED_EDGE ( 'NONE', *, *, #11343, .F. ) ;
#930 = ADVANCED_FACE ( 'NONE', ( #16471 ), #2319, .F. ) ;
#931 = AXIS2_PLACEMENT_3D ( 'NONE', #2693, #16741, #2591 ) ;
#933 = ORIENTED_EDGE ( 'NONE', *, *, #19168, .F. ) ;
#932 = VECTOR ( 'NONE', #17872, 1000.000000000000000 ) ;
#934 = LINE ( 'NONE', #13537, #8717 ) ;
#935 = CYLINDRICAL_SURFACE ( 'NONE', #8557, 4.999999999999997335 ) ;
#936 = ORIENTED_EDGE ( 'NONE', *, *, #5252, .T. ) ;
#937 = DIRECTION ( 'NONE',  ( 0.000000000000000000, 0.000000000000000000, 1.000000000000000000 ) ) ;
#938 = SURFACE_SIDE_STYLE ('',( #10546 ) ) ;
#939 = PRESENTATION_STYLE_ASSIGNMENT (( #3960 ) ) ;
#940 = CYLINDRICAL_SURFACE ( 'NONE', #16966, 1.000000000000000888 ) ;
#941 = CYLINDRICAL_SURFACE ( 'NONE', #14288, 4.000000000000007105 ) ;
#942 = PLANE ( 'NONE',  #2598 ) ;
#943 = CARTESIAN_POINT ( 'NONE',  ( -40.00000000000000000, 68.00000000000000000, 26.00000000000000355 ) ) ;
#944 = EDGE_LOOP ( 'NONE', ( #19895, #6030, #14541, #6367, #11037, #14112, #4467, #2193, #1727, #10650, #9732, #9960, #16124, #7904, #18485, #9733 ) ) ;
#945 =( NAMED_UNIT ( * ) SI_UNIT ( $, .STERADIAN. ) SOLID_ANGLE_UNIT ( ) );
#946 = LINE ( 'NONE', #5713, #10536 ) ;
#947 =( NAMED_UNIT ( * ) SI_UNIT ( $, .STERADIAN. ) SOLID_ANGLE_UNIT ( ) );
#948 = DIRECTION ( 'NONE',  ( 0.000000000000000000, 0.000000000000000000, 1.000000000000000000 ) ) ;
#949 = VECTOR ( 'NONE', #10406, 1000.000000000000000 ) ;
#950 = EDGE_CURVE ( 'NONE', #6573, #15498, #5633, .T. ) ;
#951 = VERTEX_POINT ( 'NONE', #4384 ) ;
#952 = ORIENTED_EDGE ( 'NONE', *, *, #15897, .F. ) ;
#953 = ORIENTED_EDGE ( 'NONE', *, *, #13467, .T. ) ;
#954 = EDGE_CURVE ( 'NONE', #3178, #10041, #19828, .T. ) ;
#955 = DIRECTION ( 'NONE',  ( 0.000000000000000000, 0.000000000000000000, -1.000000000000000000 ) ) ;
#956 = EDGE_LOOP ( 'NONE', ( #11937, #5518, #5980, #6334 ) ) ;
#957 = DIRECTION ( 'NONE',  ( -1.000000000000000000, -0.000000000000000000, -1.135258727068399668E-15 ) ) ;
#958 = CIRCLE ( 'NONE', #12845, 0.5249999999999994671 ) ;
#959 = ORIENTED_EDGE ( 'NONE', *, *, #2434, .F. ) ;
#960 = MECHANICAL_DESIGN_GEOMETRIC_PRESENTATION_REPRESENTATION (  '', ( #5921 ), #18084 ) ;
#961 = DIRECTION ( 'NONE',  ( -0.000000000000000000, 0.000000000000000000, 1.000000000000000000 ) ) ;
#962 = LINE ( 'NONE', #7292, #8627 ) ;
#963 = DIRECTION ( 'NONE',  ( -0.000000000000000000, -1.000000000000000000, -0.000000000000000000 ) ) ;
#964 = LINE ( 'NONE', #13573, #9811 ) ;
#965 = DIRECTION ( 'NONE',  ( -1.000000000000000000, -0.000000000000000000, 0.000000000000000000 ) ) ;
#966 = LINE ( 'NONE', #2843, #15588 ) ;
#967 = DIRECTION ( 'NONE',  ( 0.000000000000000000, 1.000000000000000000, -0.000000000000000000 ) ) ;
#968 = DIRECTION ( 'NONE',  ( 0.000000000000000000, -1.000000000000000000, 0.000000000000000000 ) ) ;
#969 = DIRECTION ( 'NONE',  ( -0.000000000000000000, -1.000000000000000000, 0.000000000000000000 ) ) ;
#970 = SURFACE_SIDE_STYLE ('',( #15127 ) ) ;
#971 = ORIENTED_EDGE ( 'NONE', *, *, #3266, .F. ) ;
#972 = AXIS2_PLACEMENT_3D ( 'NONE', #4841, #17486, #1715 ) ;
#973 = PRESENTATION_LAYER_ASSIGNMENT (  '', '', ( #20064 ) ) ;
#974 = CIRCLE ( 'NONE', #10832, 3.300000000000004263 ) ;
#975 = VERTEX_POINT ( 'NONE', #7190 ) ;
#976 = UNCERTAINTY_MEASURE_WITH_UNIT (LENGTH_MEASURE( 1.000000000000000082E-05 ), #19729, 'distance_accuracy_value', 'NONE');
#977 = ORIENTED_EDGE ( 'NONE', *, *, #9541, .F. ) ;
#978 = EDGE_CURVE ( 'NONE', #19144, #11820, #1160, .T. ) ;
#979 = CIRCLE ( 'NONE', #13853, 1.000000000000015987 ) ;
#980 = ORIENTED_EDGE ( 'NONE', *, *, #20075, .F. ) ;
#981 = CARTESIAN_POINT ( 'NONE',  ( 22.99999999999998224, 10.00000000000000000, 37.00000000000000711 ) ) ;
#982 = FACE_BOUND ( 'NONE', #19326, .T. ) ;
#983 = DIRECTION ( 'NONE',  ( -0.000000000000000000, -1.000000000000000000, -0.000000000000000000 ) ) ;
#984 = LINE ( 'NONE', #7121, #16144 ) ;
#985 = CIRCLE ( 'NONE', #10894, 1.000000000000000888 ) ;
#986 = DIRECTION ( 'NONE',  ( 1.000000000000000000, 0.000000000000000000, -0.000000000000000000 ) ) ;
#987 = CIRCLE ( 'NONE', #7596, 2.500000000000002220 ) ;
#988 = PRESENTATION_STYLE_ASSIGNMENT (( #7313 ) ) ;
#989 = FACE_OUTER_BOUND ( 'NONE', #20233, .T. ) ;
#990 = FILL_AREA_STYLE ('',( #15565 ) ) ;
#991 = FILL_AREA_STYLE_COLOUR ( '', #3961 ) ;
#992 = DIRECTION ( 'NONE',  ( 1.000000000000000000, 9.815121534730717399E-17, -0.000000000000000000 ) ) ;
#993 = DIRECTION ( 'NONE',  ( -1.000000000000000000, -2.135044278125301096E-16, -0.000000000000000000 ) ) ;
#994 = AXIS2_PLACEMENT_3D ( 'NONE', #4735, #17489, #9561 ) ;
#995 = VERTEX_POINT ( 'NONE', #13761 ) ;
#996 = AXIS2_PLACEMENT_3D ( 'NONE', #2680, #13520, #9273 ) ;
#997 = EDGE_LOOP ( 'NONE', ( #19667, #16150 ) ) ;
#998 = EDGE_LOOP ( 'NONE', ( #3956, #2228, #1884, #18628, #12737, #11202, #1629, #3238, #17351, #5028, #16860, #14048, #15733, #15344, #1597, #11329 ) ) ;
#999 = ORIENTED_EDGE ( 'NONE', *, *, #2461, .F. ) ;
#1000 = DIRECTION ( 'NONE',  ( 0.000000000000000000, -0.000000000000000000, 1.000000000000000000 ) ) ;
#1001 = UNCERTAINTY_MEASURE_WITH_UNIT (LENGTH_MEASURE( 1.000000000000000082E-05 ), #13552, 'distance_accuracy_value', 'NONE');
#1002 = EDGE_CURVE ( 'NONE', #10163, #19309, #15997, .T. ) ;
#1003 = LINE ( 'NONE', #9086, #7299 ) ;
#1004 =( REPRESENTATION_RELATIONSHIP ('NONE','NONE', #12483, #3934 ) REPRESENTATION_RELATIONSHIP_WITH_TRANSFORMATION ( #15821 )SHAPE_REPRESENTATION_RELATIONSHIP( ) );
#1005 = DIRECTION ( 'NONE',  ( -0.000000000000000000, 0.000000000000000000, 1.000000000000000000 ) ) ;
#1006 = LINE ( 'NONE', #19380, #10401 ) ;
#1007 = SURFACE_STYLE_USAGE ( .BOTH. , #19861 ) ;
#1008 = CARTESIAN_POINT ( 'NONE',  ( 503.8334540492693918, 191.8198460455371333, 168.2339398819845826 ) ) ;
#1009 = ADVANCED_FACE ( 'NONE', ( #12037 ), #19722, .F. ) ;
#1010 = SURFACE_SIDE_STYLE ('',( #4041 ) ) ;
#1011 = VECTOR ( 'NONE', #15229, 1000.000000000000000 ) ;
#1012 = FACE_OUTER_BOUND ( 'NONE', #5998, .T. ) ;
#1013 = CYLINDRICAL_SURFACE ( 'NONE', #11952, 10.00000000000000888 ) ;
#1014 = LINE ( 'NONE', #18140, #17455 ) ;
#1015 = DIRECTION ( 'NONE',  ( 0.000000000000000000, 7.137148015447440312E-15, -1.000000000000000000 ) ) ;
#1016 = ORIENTED_EDGE ( 'NONE', *, *, #6617, .F. ) ;
#1017 = CARTESIAN_POINT ( 'NONE',  ( 111.4893729001366012, 125.7247684487574588, 254.0000000000000000 ) ) ;
#1018 = DIRECTION ( 'NONE',  ( 1.000000000000000000, 0.000000000000000000, 0.000000000000000000 ) ) ;
#1019 = CARTESIAN_POINT ( 'NONE',  ( 1.399999999999999911, 13.62500000000000000, 0.000000000000000000 ) ) ;
#1020 = EDGE_CURVE ( 'NONE', #13941, #9832, #16681, .T. ) ;
#1021 = VERTEX_POINT ( 'NONE', #2533 ) ;
#1022 = VECTOR ( 'NONE', #17706, 1000.000000000000000 ) ;
#1023 = UNCERTAINTY_MEASURE_WITH_UNIT (LENGTH_MEASURE( 1.000000000000000082E-05 ), #15714, 'distance_accuracy_value', 'NONE');
#1024 = EDGE_CURVE ( 'NONE', #9760, #13294, #8830, .T. ) ;
#1025 = ORIENTED_EDGE ( 'NONE', *, *, #7894, .T. ) ;
#1026 = DIRECTION ( 'NONE',  ( -0.000000000000000000, 0.000000000000000000, 1.000000000000000000 ) ) ;
#1027 = CARTESIAN_POINT ( 'NONE',  ( -34.99999999999999289, 11.00000000000000000, 35.00000000000000711 ) ) ;
#1028 = UNCERTAINTY_MEASURE_WITH_UNIT (LENGTH_MEASURE( 1.000000000000000082E-05 ), #3866, 'distance_accuracy_value', 'NONE');
#1029 = VERTEX_POINT ( 'NONE', #15743 ) ;
#1030 = CARTESIAN_POINT ( 'NONE',  ( -31.00000000000000000, 11.00000000000000000, 25.99999999999999645 ) ) ;
#1031 = DIRECTION ( 'NONE',  ( -0.000000000000000000, 0.000000000000000000, 1.000000000000000000 ) ) ;
#1032 = CARTESIAN_POINT ( 'NONE',  ( 3.215259230344088024E-13, 140.4048636633015406, 499.8237260975782874 ) ) ;
#1033 = AXIS2_PLACEMENT_3D ( 'NONE', #6804, #489, #6898 ) ;
#1034 = EDGE_CURVE ( 'NONE', #17019, #15858, #12629, .T. ) ;
#1035 = LINE ( 'NONE', #16950, #8368 ) ;
#1036 = EDGE_CURVE ( 'NONE', #12344, #4262, #4496, .T. ) ;
#1037 =( NAMED_UNIT ( * ) SI_UNIT ( $, .STERADIAN. ) SOLID_ANGLE_UNIT ( ) );
#1038 = DIRECTION ( 'NONE',  ( 1.000000000000000000, -0.000000000000000000, 0.000000000000000000 ) ) ;
#1039 = ORIENTED_EDGE ( 'NONE', *, *, #16196, .F. ) ;
#1040 = CARTESIAN_POINT ( 'NONE',  ( 0.000000000000000000, 167.9162550801369491, -97.94896630388704750 ) ) ;
#1041 = CONICAL_SURFACE ( 'NONE', #10948, 18.17500000000000071, 0.7483780475235185525 ) ;
#1042 = PLANE ( 'NONE',  #111 ) ;
#1043 = APPLICATION_PROTOCOL_DEFINITION ( 'draft international standard', 'automotive_design', 1998, #3930 ) ;
#1044 = EDGE_CURVE ( 'NONE', #8848, #15257, #17264, .T. ) ;
#1045 = ORIENTED_EDGE ( 'NONE', *, *, #16350, .T. ) ;
#1046 = CARTESIAN_POINT ( 'NONE',  ( -41.50085094405407915, 175.4489062796178871, 505.3921618609452935 ) ) ;
#1047 = COLOUR_RGB ( '', 0.72549020, 0.75294118, 0.79215686) ;
#1048 = EDGE_CURVE ( 'NONE', #11912, #17994, #3154, .T. ) ;
#1049 = ORIENTED_EDGE ( 'NONE', *, *, #220, .T. ) ;
#1050 = EDGE_LOOP ( 'NONE', ( #9283, #18605, #18506, #2187 ) ) ;
#1051 = VECTOR ( 'NONE', #10624, 1000.000000000000000 ) ;
#1052 = ORIENTED_EDGE ( 'NONE', *, *, #9885, .F. ) ;
#1053 = DIRECTION ( 'NONE',  ( 0.000000000000000000, 0.000000000000000000, -1.000000000000000000 ) ) ;
#1054 = EDGE_LOOP ( 'NONE', ( #19573, #8675, #19299, #7566 ) ) ;
#1055 = CARTESIAN_POINT ( 'NONE',  ( -31.00000000000003197, 0.000000000000000000, 26.00000000000000355 ) ) ;
#1056 = DIRECTION ( 'NONE',  ( 0.000000000000000000, -0.000000000000000000, 1.000000000000000000 ) ) ;
#1057 = AXIS2_PLACEMENT_3D ( 'NONE', #6619, #7198, #5069 ) ;
#1058 = VERTEX_POINT ( 'NONE', #3350 ) ;
#1059 = SURFACE_STYLE_FILL_AREA ( #13567 ) ;
#1060 = SURFACE_SIDE_STYLE ('',( #2835 ) ) ;
#1061 = DIRECTION ( 'NONE',  ( -0.003530072958128175308, -0.9999937692730440641, -1.224639168707530015E-16 ) ) ;
#1062 = CARTESIAN_POINT ( 'NONE',  ( 0.000000000000000000, 145.9162550801369491, 0.000000000000000000 ) ) ;
#1063 = CLOSED_SHELL ( 'NONE', ( #8010, #12465, #4658, #16452, #19670, #16014, #5113, #14788, #8119, #16397 ) ) ;
#1064 = CIRCLE ( 'NONE', #18195, 4.999999999999997335 ) ;
#1065 = DIRECTION ( 'NONE',  ( -0.000000000000000000, -0.000000000000000000, 1.000000000000000000 ) ) ;
#1066 = EDGE_CURVE ( 'NONE', #6497, #17040, #9434, .T. ) ;
#1067 = DIRECTION ( 'NONE',  ( 0.000000000000000000, 0.000000000000000000, 1.000000000000000000 ) ) ;
#1068 = DIRECTION ( 'NONE',  ( -1.000000000000000000, 0.000000000000000000, 6.982962677686266711E-15 ) ) ;
#1069 = SURFACE_SIDE_STYLE ('',( #16782 ) ) ;
#1070 = EDGE_CURVE ( 'NONE', #5483, #14347, #11084, .T. ) ;
#1071 = CARTESIAN_POINT ( 'NONE',  ( -81.18192946989245229, 138.7545334744432637, 491.0690926367356042 ) ) ;
#1072 = DIRECTION ( 'NONE',  ( -1.000000000000000000, -0.000000000000000000, -0.000000000000000000 ) ) ;
#1073 = PRESENTATION_LAYER_ASSIGNMENT (  '', '', ( #8668 ) ) ;
#1074 = ORIENTED_EDGE ( 'NONE', *, *, #13658, .F. ) ;
#1075 = VECTOR ( 'NONE', #13463, 1000.000000000000000 ) ;
#1076 = EDGE_CURVE ( 'NONE', #11219, #16393, #1461, .T. ) ;
#1077 = ORIENTED_EDGE ( 'NONE', *, *, #16118, .T. ) ;
#1078 = ORIENTED_EDGE ( 'NONE', *, *, #5608, .F. ) ;
#1079 = VECTOR ( 'NONE', #12004, 1000.000000000000000 ) ;
#1080 = AXIS2_PLACEMENT_3D ( 'NONE', #15697, #15784, #1522 ) ;
#1081 = ORIENTED_EDGE ( 'NONE', *, *, #13213, .T. ) ;
#1082 = LINE ( 'NONE', #7417, #17652 ) ;
#1083 = AXIS2_PLACEMENT_3D ( 'NONE', #646, #16252, #11584 ) ;
#1084 = ORIENTED_EDGE ( 'NONE', *, *, #13899, .F. ) ;
#1085 = CARTESIAN_POINT ( 'NONE',  ( 111.4893729001366012, 127.7247684487574588, 254.0000000000000000 ) ) ;
#1086 = FACE_OUTER_BOUND ( 'NONE', #15879, .T. ) ;
#1087 = CARTESIAN_POINT ( 'NONE',  ( 40.00000000000000000, 68.00000000000000000, -25.99999999999999645 ) ) ;
#1088 = MECHANICAL_DESIGN_GEOMETRIC_PRESENTATION_REPRESENTATION (  '', ( #4747 ), #9015 ) ;
#1089 = FACE_BOUND ( 'NONE', #14856, .T. ) ;
#1090 = AXIS2_PLACEMENT_3D ( 'NONE', #7561, #20225, #18161 ) ;
#1091 = LINE ( 'NONE', #4225, #11403 ) ;
#1092 = LINE ( 'NONE', #7612, #18888 ) ;
#1093 = STYLED_ITEM ( 'NONE', ( #4255 ), #15737 ) ;
#1094 = CARTESIAN_POINT ( 'NONE',  ( -211.5106270998635409, 103.1299228374912360, 79.58252780074349175 ) ) ;
#1095 =( LENGTH_UNIT ( ) NAMED_UNIT ( * ) SI_UNIT ( .MILLI., .METRE. ) );
#1096 = SURFACE_STYLE_USAGE ( .BOTH. , #10502 ) ;
#1097 =( GEOMETRIC_REPRESENTATION_CONTEXT ( 3 ) GLOBAL_UNCERTAINTY_ASSIGNED_CONTEXT ( ( #2702 ) ) GLOBAL_UNIT_ASSIGNED_CONTEXT ( ( #7069, #15808, #7770 ) ) REPRESENTATION_CONTEXT ( 'NONE', 'WORKASPACE' ) );
#1098 = EDGE_CURVE ( 'NONE', #5632, #693, #1571, .T. ) ;
#1099 = CIRCLE ( 'NONE', #14624, 10.00000000000000888 ) ;
#1100 = DIRECTION ( 'NONE',  ( -0.000000000000000000, -1.000000000000000000, -0.000000000000000000 ) ) ;
#1101 = DIRECTION ( 'NONE',  ( 0.000000000000000000, 0.000000000000000000, -1.000000000000000000 ) ) ;
#1102 = VECTOR ( 'NONE', #14007, 1000.000000000000000 ) ;
#1103 = AXIS2_PLACEMENT_3D ( 'NONE', #2099, #16261, #10058 ) ;
#1104 = VECTOR ( 'NONE', #4019, 1000.000000000000000 ) ;
#1105 = EDGE_LOOP ( 'NONE', ( #11410, #14369, #14768, #14708 ) ) ;
#1106 = AXIS2_PLACEMENT_3D ( 'NONE', #16736, #20301, #12584 ) ;
#1107 = ORIENTED_EDGE ( 'NONE', *, *, #2833, .F. ) ;
#1108 = AXIS2_PLACEMENT_3D ( 'NONE', #5274, #19282, #17730 ) ;
#1109 = CARTESIAN_POINT ( 'NONE',  ( 498.8334540492693918, 191.8198460455371333, 81.76606011801540319 ) ) ;
#1110 = ORIENTED_EDGE ( 'NONE', *, *, #4493, .F. ) ;
#1111 = ORIENTED_EDGE ( 'NONE', *, *, #7761, .F. ) ;
#1112 = CARTESIAN_POINT ( 'NONE',  ( 10.00000000000000000, 372.8685141053783241, -143.5198051533979537 ) ) ;
#1113 = DIRECTION ( 'NONE',  ( 1.000000000000000000, 0.000000000000000000, 0.000000000000000000 ) ) ;
#1114 = CARTESIAN_POINT ( 'NONE',  ( -211.5106270998635409, 113.1299228374912502, 79.58252780074349175 ) ) ;
#1115 = CARTESIAN_POINT ( 'NONE',  ( 423.8334540492694487, 191.8198460455371333, 24.99421986894476078 ) ) ;
#1116 = CARTESIAN_POINT ( 'NONE',  ( -211.5106270998635409, 123.1299228374912644, 220.6387154965113382 ) ) ;
#1117 =( LENGTH_UNIT ( ) NAMED_UNIT ( * ) SI_UNIT ( .MILLI., .METRE. ) );
#1118 = CARTESIAN_POINT ( 'NONE',  ( 39.99999999999999289, 8.000000000000000000, 26.00000000000000000 ) ) ;
#1119 = AXIS2_PLACEMENT_3D ( 'NONE', #10554, #15097, #13250 ) ;
#1120 = DIRECTION ( 'NONE',  ( 0.000000000000000000, 0.000000000000000000, -1.000000000000000000 ) ) ;
#1121 = CARTESIAN_POINT ( 'NONE',  ( -38.50085094405407204, 159.0821755739672483, 505.3921618609452935 ) ) ;
#1122 = CARTESIAN_POINT ( 'NONE',  ( -80.85993302188293796, 138.8314847507810725, 489.5655098117073862 ) ) ;
#1123 = VECTOR ( 'NONE', #9946, 1000.000000000000000 ) ;
#1124 = LINE ( 'NONE', #6288, #3032 ) ;
#1125 = ORIENTED_EDGE ( 'NONE', *, *, #2982, .F. ) ;
#1126 = SURFACE_STYLE_FILL_AREA ( #18353 ) ;
#1127 = COLOUR_RGB ( '', 0.31764706, 0.68627451, 0.89019608) ;
#1128 = CONICAL_SURFACE ( 'NONE', #13367, 0.9999999999999950040, 1.029744258676644320 ) ;
#1129 = PRODUCT_DEFINITION ( 'UNKNOWN', '', #19816, #15036 ) ;
#1130 = ORIENTED_EDGE ( 'NONE', *, *, #7791, .F. ) ;
#1131 = ORIENTED_EDGE ( 'NONE', *, *, #1411, .F. ) ;
#1132 = EDGE_CURVE ( 'NONE', #566, #3836, #6778, .T. ) ;
#1133 = DIRECTION ( 'NONE',  ( 0.000000000000000000, 0.000000000000000000, 1.000000000000000000 ) ) ;
#1134 = CARTESIAN_POINT ( 'NONE',  ( 1.181929469892549323, 139.7545334744432637, 491.0690926367356042 ) ) ;
#1135 = ORIENTED_EDGE ( 'NONE', *, *, #19807, .F. ) ;
#1136 = CARTESIAN_POINT ( 'NONE',  ( 149.0892156028631348, 167.9162550801369491, 245.0000000000000000 ) ) ;
#1137 = CARTESIAN_POINT ( 'NONE',  ( -79.63624027127092120, 139.7550675453751694, 500.7965084021044504 ) ) ;
#1138 = VECTOR ( 'NONE', #6526, 1000.000000000000000 ) ;
#1139 = STYLED_ITEM ( 'NONE', ( #5982 ), #9261 ) ;
#1140 = DIRECTION ( 'NONE',  ( 0.000000000000000000, 0.000000000000000000, 1.000000000000000000 ) ) ;
#1141 = DIRECTION ( 'NONE',  ( 9.815121534730717399E-17, -1.000000000000000000, 0.000000000000000000 ) ) ;
#1142 = ORIENTED_EDGE ( 'NONE', *, *, #9857, .F. ) ;
#1143 = PRODUCT_CONTEXT ( 'NONE', #2078, 'mechanical' ) ;
#1144 = EDGE_CURVE ( 'NONE', #19923, #666, #17154, .T. ) ;
#1145 = VERTEX_POINT ( 'NONE', #15640 ) ;
#1146 = ORIENTED_EDGE ( 'NONE', *, *, #16628, .T. ) ;
#1147 = FILL_AREA_STYLE ('',( #15312 ) ) ;
#1148 = ORIENTED_EDGE ( 'NONE', *, *, #13345, .F. ) ;
#1149 = ORIENTED_EDGE ( 'NONE', *, *, #15445, .T. ) ;
#1150 = COLOUR_RGB ( '', 0.31764706, 0.68627451, 0.89019608) ;
#1151 = ADVANCED_FACE ( 'NONE', ( #9220 ), #14267, .F. ) ;
#1152 = ORIENTED_EDGE ( 'NONE', *, *, #4980, .T. ) ;
#1153 = CIRCLE ( 'NONE', #12722, 36.50000000000000000 ) ;
#1154 = ADVANCED_FACE ( 'NONE', ( #18993 ), #4899, .F. ) ;
#1155 = DIRECTION ( 'NONE',  ( 0.000000000000000000, -0.7071067811865494601, 0.7071067811865456854 ) ) ;
#1156 = EDGE_LOOP ( 'NONE', ( #18013, #5005, #16057, #12621 ) ) ;
#1157 = DIRECTION ( 'NONE',  ( -0.000000000000000000, -1.000000000000000000, -0.000000000000000000 ) ) ;
#1158 = CARTESIAN_POINT ( 'NONE',  ( -3.000000000000000000, -1.836909530733565148E-16, 22.00000000000000000 ) ) ;
#1159 = CIRCLE ( 'NONE', #12731, 10.00000000000000888 ) ;
#1160 = LINE ( 'NONE', #6041, #1791 ) ;
#1161 =( NAMED_UNIT ( * ) PLANE_ANGLE_UNIT ( ) SI_UNIT ( $, .RADIAN. ) );
#1162 = EDGE_CURVE ( 'NONE', #15503, #2504, #16325, .T. ) ;
#1163 = CARTESIAN_POINT ( 'NONE',  ( -22.00000000000001776, 8.000000000000000000, 33.00000000000000711 ) ) ;
#1164 = CARTESIAN_POINT ( 'NONE',  ( 108.9893729001366012, 144.5787140289007766, 293.4524157190247138 ) ) ;
#1165 = CARTESIAN_POINT ( 'NONE',  ( 111.4893729001366012, 127.7247684487574588, 254.0000000000000000 ) ) ;
#1166 = AXIS2_PLACEMENT_3D ( 'NONE', #18221, #7216, #2239 ) ;
#1167 = FILL_AREA_STYLE_COLOUR ( '', #3110 ) ;
#1168 = DIRECTION ( 'NONE',  ( 0.000000000000000000, 1.000000000000000000, -0.000000000000000000 ) ) ;
#1169 = FACE_OUTER_BOUND ( 'NONE', #7881, .T. ) ;
#1170 = PLANE ( 'NONE',  #735 ) ;
#1171 = STYLED_ITEM ( 'NONE', ( #13407 ), #9595 ) ;
#1172 = CARTESIAN_POINT ( 'NONE',  ( 2.265596578422603396E-15, 19.00100000000000122, 18.50000000000000000 ) ) ;
#1173 = DIRECTION ( 'NONE',  ( 0.000000000000000000, 2.352167425053297897E-16, 1.000000000000000000 ) ) ;
#1174 = DIRECTION ( 'NONE',  ( 0.000000000000000000, 0.000000000000000000, 1.000000000000000000 ) ) ;
#1175 = EDGE_CURVE ( 'NONE', #4977, #1058, #16445, .T. ) ;
#1176 = CARTESIAN_POINT ( 'NONE',  ( 1.181929469891187301, 216.7545334744432921, 489.5655098179833544 ) ) ;
#1177 = CARTESIAN_POINT ( 'NONE',  ( 40.00000000000000711, 0.000000000000000000, 34.99999999999997868 ) ) ;
#1178 = ORIENTED_EDGE ( 'NONE', *, *, #11437, .F. ) ;
#1179 = ORIENTED_EDGE ( 'NONE', *, *, #5983, .T. ) ;
#1180 = EDGE_CURVE ( 'NONE', #4081, #18280, #14650, .T. ) ;
#1181 = EDGE_LOOP ( 'NONE', ( #100, #4789, #10034, #9950 ) ) ;
#1182 = ORIENTED_EDGE ( 'NONE', *, *, #10165, .F. ) ;
#1183 = EDGE_LOOP ( 'NONE', ( #3020, #10540 ) ) ;
#1184 = FACE_OUTER_BOUND ( 'NONE', #17712, .T. ) ;
#1185 =( NAMED_UNIT ( * ) PLANE_ANGLE_UNIT ( ) SI_UNIT ( $, .RADIAN. ) );
#1186 = CARTESIAN_POINT ( 'NONE',  ( 109.4893729001366012, 129.7247684487574588, 370.0000000000000000 ) ) ;
#1187 = ORIENTED_EDGE ( 'NONE', *, *, #11079, .T. ) ;
#1188 = DIRECTION ( 'NONE',  ( -0.000000000000000000, 1.000000000000000000, 1.632680918566406547E-16 ) ) ;
#1189 = DIRECTION ( 'NONE',  ( 1.000000000000000000, 0.000000000000000000, -0.000000000000000000 ) ) ;
#1190 = SURFACE_STYLE_USAGE ( .BOTH. , #18419 ) ;
#1191 = PLANE ( 'NONE',  #16362 ) ;
#1192 = DIRECTION ( 'NONE',  ( 3.854941057726254367E-16, 0.000000000000000000, 1.000000000000000000 ) ) ;
#1193 = CARTESIAN_POINT ( 'NONE',  ( -8.881784197001250351E-16, 0.000000000000000000, 0.000000000000000000 ) ) ;
#1194 =( NAMED_UNIT ( * ) PLANE_ANGLE_UNIT ( ) SI_UNIT ( $, .RADIAN. ) );
#1195 = CARTESIAN_POINT ( 'NONE',  ( -40.00000000000000000, 19.00000000000000000, -26.00000000000000355 ) ) ;
#1196 = AXIS2_PLACEMENT_3D ( 'NONE', #211, #6615, #13119 ) ;
#1197 = PRESENTATION_STYLE_ASSIGNMENT (( #11962 ) ) ;
#1198 = ADVANCED_FACE ( 'NONE', ( #19104 ), #453, .T. ) ;
#1199 = ORIENTED_EDGE ( 'NONE', *, *, #16993, .F. ) ;
#1200 = ORIENTED_EDGE ( 'NONE', *, *, #12080, .T. ) ;
#1201 =( NAMED_UNIT ( * ) SI_UNIT ( $, .STERADIAN. ) SOLID_ANGLE_UNIT ( ) );
#1202 = ORIENTED_EDGE ( 'NONE', *, *, #15177, .F. ) ;
#1203 = ORIENTED_EDGE ( 'NONE', *, *, #10783, .F. ) ;
#1204 = STYLED_ITEM ( 'NONE', ( #4420 ), #12124 ) ;
#1205 = CARTESIAN_POINT ( 'NONE',  ( -79.99999999999995737, 152.4824555358011082, 486.3411705753778165 ) ) ;
#1206 = EDGE_LOOP ( 'NONE', ( #17914, #14852, #575, #8505 ) ) ;
#1207 = CARTESIAN_POINT ( 'NONE',  ( -22.99999999999999645, 68.00000000000000000, -36.99999999999999289 ) ) ;
#1208 = UNCERTAINTY_MEASURE_WITH_UNIT (LENGTH_MEASURE( 1.000000000000000082E-05 ), #12422, 'distance_accuracy_value', 'NONE');
#1209 = AXIS2_PLACEMENT_3D ( 'NONE', #11207, #77, #12560 ) ;
#1210 = CARTESIAN_POINT ( 'NONE',  ( 0.000000000000000000, 309.2289037985890445, -150.1198051533984597 ) ) ;
#1211 = FILL_AREA_STYLE ('',( #15377 ) ) ;
#1212 = CYLINDRICAL_SURFACE ( 'NONE', #20170, 5.000000000000000888 ) ;
#1213 = DIRECTION ( 'NONE',  ( -0.000000000000000000, -1.000000000000000000, -0.000000000000000000 ) ) ;
#1214 =( NAMED_UNIT ( * ) SI_UNIT ( $, .STERADIAN. ) SOLID_ANGLE_UNIT ( ) );
#1215 = FILL_AREA_STYLE ('',( #3306 ) ) ;
#1216 = ORIENTED_EDGE ( 'NONE', *, *, #5858, .F. ) ;
#1217 = PLANE ( 'NONE',  #8212 ) ;
#1218 = FACE_OUTER_BOUND ( 'NONE', #1856, .T. ) ;
#1219 = VECTOR ( 'NONE', #13981, 1000.000000000000000 ) ;
#1220 = EDGE_LOOP ( 'NONE', ( #20096, #14071, #18783, #7511 ) ) ;
#1221 = EDGE_CURVE ( 'NONE', #5719, #8487, #19218, .T. ) ;
#1222 = ORIENTED_EDGE ( 'NONE', *, *, #14307, .F. ) ;
#1223 = LINE ( 'NONE', #15501, #19542 ) ;
#1224 = FACE_BOUND ( 'NONE', #11623, .T. ) ;
#1225 = ORIENTED_EDGE ( 'NONE', *, *, #9468, .F. ) ;
#1226 = DIRECTION ( 'NONE',  ( 0.000000000000000000, 0.000000000000000000, 1.000000000000000000 ) ) ;
#1227 = MANIFOLD_SOLID_BREP ( 'Boss-Extrude4', #14918 ) ;
#1228 = SURFACE_STYLE_FILL_AREA ( #10749 ) ;
#1229 = VECTOR ( 'NONE', #18980, 1000.000000000000000 ) ;
#1230 = DIRECTION ( 'NONE',  ( -1.000000000000000000, -0.000000000000000000, -0.000000000000000000 ) ) ;
#1231 = DIRECTION ( 'NONE',  ( 1.000000000000000000, -0.000000000000000000, 0.000000000000000000 ) ) ;
#1232 = CARTESIAN_POINT ( 'NONE',  ( 31.00000000000002842, 68.00000000000000000, 26.00000000000001066 ) ) ;
#1233 = ORIENTED_EDGE ( 'NONE', *, *, #4236, .F. ) ;
#1234 = CYLINDRICAL_SURFACE ( 'NONE', #19677, 10.00000000000000888 ) ;
#1235 =( LENGTH_UNIT ( ) NAMED_UNIT ( * ) SI_UNIT ( .MILLI., .METRE. ) );
#1236 = FILL_AREA_STYLE_COLOUR ( '', #12312 ) ;
#1237 = APPLICATION_PROTOCOL_DEFINITION ( 'draft international standard', 'automotive_design', 1998, #2487 ) ;
#1238 = ORIENTED_EDGE ( 'NONE', *, *, #15682, .T. ) ;
#1239 = ORIENTED_EDGE ( 'NONE', *, *, #10264, .T. ) ;
#1240 = EDGE_CURVE ( 'NONE', #15834, #7815, #17674, .T. ) ;
#1241 = ORIENTED_EDGE ( 'NONE', *, *, #4726, .T. ) ;
#1243 = VERTEX_POINT ( 'NONE', #14690 ) ;
#1242 =( BOUNDED_SURFACE ( )  B_SPLINE_SURFACE ( 3, 2, ( 
 ( #3172, #15860, #14189 ),
 ( #17694, #177, #3373 ),
 ( #6577, #9453, #4714 ),
 ( #15762, #8325, #12869 ),
 ( #8219, #17478, #12549 ),
 ( #17591, #1590, #7910 ),
 ( #16177, #11005, #12659 ),
 ( #6273, #9652, #6374 ),
 ( #65, #18925, #2005 ),
 ( #20361, #19126, #4828 ),
 ( #15979, #11102, #17288 ),
 ( #17384, #1819, #4920 ),
 ( #3269, #3583, #14494 ),
 ( #11200, #6474, #18812 ) ),
 .UNSPECIFIED., .F., .F., .T. ) 
 B_SPLINE_SURFACE_WITH_KNOTS ( ( 4, 2, 2, 2, 2, 2, 4 ),
 ( 3, 3 ),
 ( 0.001011094481076133932, 0.001870411825472422613, 0.002300070497670567062, 0.002729729169868711294, 0.003159387842066855526, 0.003589046514264999758, 0.004448363858661288223 ),
 ( 0.000000000000000000, 1.000000000000000000 ),
 .UNSPECIFIED. ) 
 GEOMETRIC_REPRESENTATION_ITEM ( )  RATIONAL_B_SPLINE_SURFACE ( (
 ( 1.000000000000000000, 0.7071067811865475727, 1.000000000000000000),
 ( 1.000000000000000000, 0.7323290926429416592, 1.000000000000000000),
 ( 1.000000000000000000, 0.7535416720974540405, 1.000000000000000000),
 ( 1.000000000000000000, 0.7799492680867576855, 1.000000000000000000),
 ( 1.000000000000000000, 0.7878446813477756328, 1.000000000000000000),
 ( 1.000000000000000000, 0.8013484601504040628, 1.000000000000000000),
 ( 1.000000000000000000, 0.8070584780280735115, 1.000000000000000000),
 ( 1.000000000000000000, 0.8167183804147478687, 1.000000000000000000),
 ( 1.000000000000000000, 0.8205285662994377116, 1.000000000000000000),
 ( 1.000000000000000000, 0.8265885805974317879, 1.000000000000000000),
 ( 1.000000000000000000, 0.8288784836241653853, 1.000000000000000000),
 ( 1.000000000000000000, 0.8339575989303936732, 1.000000000000000000),
 ( 1.000000000000000000, 0.8350775064303027628, 1.000000000000000000),
 ( 1.000000000000000000, 0.8351454326190045352, 1.000000000000000000) ) ) 
 REPRESENTATION_ITEM ( '' )  SURFACE ( )  );
#1244 = VECTOR ( 'NONE', #5317, 1000.000000000000000 ) ;
#1245 = ORIENTED_EDGE ( 'NONE', *, *, #20310, .T. ) ;
#1246 = FACE_OUTER_BOUND ( 'NONE', #17359, .T. ) ;
#1247 = VERTEX_POINT ( 'NONE', #8586 ) ;
#1248 = FACE_OUTER_BOUND ( 'NONE', #5306, .T. ) ;
#1249 = EDGE_CURVE ( 'NONE', #13405, #11940, #5119, .T. ) ;
#1250 = DIRECTION ( 'NONE',  ( 3.854941057726249930E-16, 0.000000000000000000, 1.000000000000000000 ) ) ;
#1251 = DIRECTION ( 'NONE',  ( 0.000000000000000000, 0.000000000000000000, 1.000000000000000000 ) ) ;
#1252 = AXIS2_PLACEMENT_3D ( 'NONE', #12885, #18942, #9259 ) ;
#1253 = DIRECTION ( 'NONE',  ( 1.000000000000000000, -0.000000000000000000, -0.000000000000000000 ) ) ;
#1254 = CARTESIAN_POINT ( 'NONE',  ( -26.00000000000002132, 10.00000000000000000, -31.00000000000003553 ) ) ;
#1255 = DIRECTION ( 'NONE',  ( 0.000000000000000000, 0.000000000000000000, -1.000000000000000000 ) ) ;
#1256 = AXIS2_PLACEMENT_3D ( 'NONE', #13287, #11739, #4107 ) ;
#1257 = DIRECTION ( 'NONE',  ( -0.000000000000000000, -1.000000000000000000, -0.000000000000000000 ) ) ;
#1258 = EDGE_CURVE ( 'NONE', #13299, #7205, #13069, .T. ) ;
#1259 = LINE ( 'NONE', #13681, #2227 ) ;
#1260 = DIRECTION ( 'NONE',  ( 0.000000000000000000, 0.000000000000000000, 1.000000000000000000 ) ) ;
#1261 = CARTESIAN_POINT ( 'NONE',  ( 35.00000000000003553, 0.000000000000000000, -23.50000000000000000 ) ) ;
#1262 =( LENGTH_UNIT ( ) NAMED_UNIT ( * ) SI_UNIT ( .MILLI., .METRE. ) );
#1263 = CARTESIAN_POINT ( 'NONE',  ( 5.941205806953520074, 0.000000000000000000, 0.000000000000000000 ) ) ;
#1264 = MANIFOLD_SOLID_BREP ( 'Imported1', #20162 ) ;
#1265 = DIRECTION ( 'NONE',  ( 0.000000000000000000, 0.000000000000000000, -1.000000000000000000 ) ) ;
#1266 = DIRECTION ( 'NONE',  ( -0.000000000000000000, 0.000000000000000000, 1.000000000000000000 ) ) ;
#1267 = DIRECTION ( 'NONE',  ( -1.000000000000000000, -0.000000000000000000, -1.156482317317870344E-15 ) ) ;
#1268 = EDGE_CURVE ( 'NONE', #14439, #5719, #11587, .T. ) ;
#1269 = ORIENTED_EDGE ( 'NONE', *, *, #14536, .F. ) ;
#1270 =( GEOMETRIC_REPRESENTATION_CONTEXT ( 3 ) GLOBAL_UNCERTAINTY_ASSIGNED_CONTEXT ( ( #8267 ) ) GLOBAL_UNIT_ASSIGNED_CONTEXT ( ( #7302, #19842, #18311 ) ) REPRESENTATION_CONTEXT ( 'NONE', 'WORKASPACE' ) );
#1271 = VECTOR ( 'NONE', #18931, 1000.000000000000000 ) ;
#1272 = ORIENTED_EDGE ( 'NONE', *, *, #5335, .F. ) ;
#1273 = COLOUR_RGB ( '', 0.66274510, 0.83137255, 0.94901961) ;
#1274 = ORIENTED_EDGE ( 'NONE', *, *, #14830, .T. ) ;
#1275 = DIRECTION ( 'NONE',  ( 1.000000000000000000, 0.000000000000000000, -0.000000000000000000 ) ) ;
#1276 = CARTESIAN_POINT ( 'NONE',  ( 475.8334540492694487, 214.2156642432025251, 245.0000000000000000 ) ) ;
#1277 = EDGE_CURVE ( 'NONE', #9315, #6242, #11702, .T. ) ;
#1278 = PRESENTATION_STYLE_ASSIGNMENT (( #16794 ) ) ;
#1279 = VERTEX_POINT ( 'NONE', #5822 ) ;
#1280 = PRESENTATION_STYLE_ASSIGNMENT (( #9062 ) ) ;
#1281 = SURFACE_STYLE_USAGE ( .BOTH. , #1392 ) ;
#1282 = CARTESIAN_POINT ( 'NONE',  ( 22.99999999999995737, 0.000000000000000000, -33.99999999999998579 ) ) ;
#1283 =( NAMED_UNIT ( * ) SI_UNIT ( $, .STERADIAN. ) SOLID_ANGLE_UNIT ( ) );
#1284 = CARTESIAN_POINT ( 'NONE',  ( 10.00000000000000000, 309.2289037985890445, -146.8198051533984199 ) ) ;
#1285 = DIRECTION ( 'NONE',  ( -0.000000000000000000, -0.000000000000000000, 1.000000000000000000 ) ) ;
#1286 =( NAMED_UNIT ( * ) SI_UNIT ( $, .STERADIAN. ) SOLID_ANGLE_UNIT ( ) );
#1287 = EDGE_CURVE ( 'NONE', #14622, #18716, #6528, .T. ) ;
#1288 = CARTESIAN_POINT ( 'NONE',  ( 53.48937290013659407, 145.9162550801369491, 250.0000000000000000 ) ) ;
#1289 = AXIS2_PLACEMENT_3D ( 'NONE', #6135, #18680, #18875 ) ;
#1290 = AXIS2_PLACEMENT_3D ( 'NONE', #14218, #14029, #13812 ) ;
#1291 = DIRECTION ( 'NONE',  ( -9.815121534730717399E-17, 1.000000000000000000, 0.000000000000000000 ) ) ;
#1292 = FILL_AREA_STYLE ('',( #15463 ) ) ;
#1293 = EDGE_CURVE ( 'NONE', #10363, #243, #10644, .T. ) ;
#1294 = VERTEX_POINT ( 'NONE', #2808 ) ;
#1295 = EDGE_CURVE ( 'NONE', #2815, #14814, #12637, .T. ) ;
#1296 = ORIENTED_EDGE ( 'NONE', *, *, #11649, .T. ) ;
#1297 = ORIENTED_EDGE ( 'NONE', *, *, #9374, .F. ) ;
#1298 = FILL_AREA_STYLE_COLOUR ( '', #7408 ) ;
#1299 = ORIENTED_EDGE ( 'NONE', *, *, #17199, .F. ) ;
#1300 = ORIENTED_EDGE ( 'NONE', *, *, #8914, .T. ) ;
#1301 = ORIENTED_EDGE ( 'NONE', *, *, #16523, .F. ) ;
#1302 = DIRECTION ( 'NONE',  ( 0.000000000000000000, 1.000000000000000000, 0.000000000000000000 ) ) ;
#1303 = AXIS2_PLACEMENT_3D ( 'NONE', #16137, #14674, #546 ) ;
#1304 =( NAMED_UNIT ( * ) SI_UNIT ( $, .STERADIAN. ) SOLID_ANGLE_UNIT ( ) );
#1305 = DIRECTION ( 'NONE',  ( 0.000000000000000000, 1.000000000000000000, 0.000000000000000000 ) ) ;
#1306 =( NAMED_UNIT ( * ) PLANE_ANGLE_UNIT ( ) SI_UNIT ( $, .RADIAN. ) );
#1307 = PRODUCT_DEFINITION_SHAPE ( 'NONE', 'NONE',  #15412 ) ;
#1308 = LINE ( 'NONE', #17410, #7361 ) ;
#1309 = DIRECTION ( 'NONE',  ( 1.595148023886719315E-16, -1.000000000000000000, 0.000000000000000000 ) ) ;
#1310 = LINE ( 'NONE', #4864, #6423 ) ;
#1311 = SURFACE_STYLE_FILL_AREA ( #9695 ) ;
#1312 = LINE ( 'NONE', #2991, #18186 ) ;
#1313 = ORIENTED_EDGE ( 'NONE', *, *, #16220, .F. ) ;
#1314 = CARTESIAN_POINT ( 'NONE',  ( 98.48937290013662960, 113.1299228374914350, 79.58252780074349175 ) ) ;
#1315 = SURFACE_STYLE_USAGE ( .BOTH. , #11987 ) ;
#1316 = ADVANCED_FACE ( 'NONE', ( #19694 ), #14623, .T. ) ;
#1317 = COLOUR_RGB ( '', 0.40784314, 0.44705882, 0.49803922) ;
#1318 = CARTESIAN_POINT ( 'NONE',  ( 25.99999999999998224, 0.000000000000000000, -31.00000000000003197 ) ) ;
#1319 = CIRCLE ( 'NONE', #16839, 1.800000000000000266 ) ;
#1320 = AXIS2_PLACEMENT_3D ( 'NONE', #20191, #19881, #5796 ) ;
#1321 = ADVANCED_FACE ( 'NONE', ( #15089 ), #18364, .F. ) ;
#1322 = ORIENTED_EDGE ( 'NONE', *, *, #798, .F. ) ;
#1323 = FACE_OUTER_BOUND ( 'NONE', #3933, .T. ) ;
#1324 = ORIENTED_EDGE ( 'NONE', *, *, #15595, .T. ) ;
#1325 = CARTESIAN_POINT ( 'NONE',  ( 423.8334540492694487, 191.8198460455371333, 215.0057801310552179 ) ) ;
#1326 = FACE_OUTER_BOUND ( 'NONE', #10310, .T. ) ;
#1327 = ORIENTED_EDGE ( 'NONE', *, *, #2827, .T. ) ;
#1328 = FILL_AREA_STYLE_COLOUR ( '', #13365 ) ;
#1329 = MANIFOLD_SOLID_BREP ( 'Cut-Extrude4[1]', #11290 ) ;
#1330 = CARTESIAN_POINT ( 'NONE',  ( 463.8334540492693350, 134.2156642432025251, 0.000000000000000000 ) ) ;
#1331 = CYLINDRICAL_SURFACE ( 'NONE', #7752, 4.999999999999997335 ) ;
#1332 = DIRECTION ( 'NONE',  ( 0.000000000000000000, 0.000000000000000000, -1.000000000000000000 ) ) ;
#1333 = DIRECTION ( 'NONE',  ( -0.000000000000000000, -1.000000000000000000, -0.000000000000000000 ) ) ;
#1334 = ORIENTED_EDGE ( 'NONE', *, *, #3903, .F. ) ;
#1335 = FACE_OUTER_BOUND ( 'NONE', #3758, .T. ) ;
#1336 = ORIENTED_EDGE ( 'NONE', *, *, #16251, .F. ) ;
#1337 = CARTESIAN_POINT ( 'NONE',  ( 53.48937290013658696, 126.1646452518344859, 322.0399576098686225 ) ) ;
#1338 = DIRECTION ( 'NONE',  ( -0.000000000000000000, -1.000000000000000000, -0.000000000000000000 ) ) ;
#1339 = APPLICATION_PROTOCOL_DEFINITION ( 'draft international standard', 'automotive_design', 1998, #4593 ) ;
#1340 = EDGE_CURVE ( 'NONE', #298, #17762, #13741, .T. ) ;
#1341 = VERTEX_POINT ( 'NONE', #20318 ) ;
#1342 = FILL_AREA_STYLE_COLOUR ( '', #1700 ) ;
#1343 = EDGE_LOOP ( 'NONE', ( #7833, #10893, #10967, #8608 ) ) ;
#1344 = VECTOR ( 'NONE', #19201, 1000.000000000000000 ) ;
#1345 = ORIENTED_EDGE ( 'NONE', *, *, #3338, .T. ) ;
#1346 = ORIENTED_EDGE ( 'NONE', *, *, #19791, .F. ) ;
#1347 = CYLINDRICAL_SURFACE ( 'NONE', #4460, 3.000000000000000888 ) ;
#1348 = AXIS2_PLACEMENT_3D ( 'NONE', #16555, #11911, #7480 ) ;
#1349 = AXIS2_PLACEMENT_3D ( 'NONE', #19256, #5337, #9870 ) ;
#1350 = VERTEX_POINT ( 'NONE', #6323 ) ;
#1351 = CARTESIAN_POINT ( 'NONE',  ( 0.07056292634023825228, 141.0639970544592927, 501.4403512417491129 ) ) ;
#1352 = DIRECTION ( 'NONE',  ( 1.000000000000000000, -0.000000000000000000, -0.000000000000000000 ) ) ;
#1353 = CARTESIAN_POINT ( 'NONE',  ( -26.00000000000002132, 10.00000000000000000, 40.00000000000000711 ) ) ;
#1354 = CARTESIAN_POINT ( 'NONE',  ( -23.00000000000003197, 3.000000000000000000, 37.00000000000000711 ) ) ;
#1355 = AXIS2_PLACEMENT_3D ( 'NONE', #16391, #495, #16189 ) ;
#1356 = AXIS2_PLACEMENT_3D ( 'NONE', #4603, #3257, #9534 ) ;
#1357 = CYLINDRICAL_SURFACE ( 'NONE', #17501, 15.25000000000000000 ) ;
#1358 = EDGE_CURVE ( 'NONE', #3349, #20011, #6222, .T. ) ;
#1359 = DIRECTION ( 'NONE',  ( 1.000000000000000000, 0.000000000000000000, 0.000000000000000000 ) ) ;
#1360 = CARTESIAN_POINT ( 'NONE',  ( 30.99999999999996092, 0.000000000000000000, -30.99999999999999289 ) ) ;
#1361 = LINE ( 'NONE', #4600, #18892 ) ;
#1362 = DIRECTION ( 'NONE',  ( -1.000000000000000000, 0.000000000000000000, 0.000000000000000000 ) ) ;
#1363 = CARTESIAN_POINT ( 'NONE',  ( 423.8334540492694487, 191.8198460455371333, 71.76606011801538898 ) ) ;
#1364 = DIRECTION ( 'NONE',  ( -0.000000000000000000, -1.000000000000000000, -0.000000000000000000 ) ) ;
#1365 = CARTESIAN_POINT ( 'NONE',  ( 23.66755185189983735, -100.1139154823664796, 76.44844828963165639 ) ) ;
#1366 = CARTESIAN_POINT ( 'NONE',  ( 31.99999999999998579, 6.000000000000000000, 22.99999999999999645 ) ) ;
#1367 = FACE_BOUND ( 'NONE', #8452, .T. ) ;
#1368 = MANIFOLD_SOLID_BREP ( 'Cut-Extrude3[3]', #4719 ) ;
#1369 =( LENGTH_UNIT ( ) NAMED_UNIT ( * ) SI_UNIT ( .MILLI., .METRE. ) );
#1370 = CIRCLE ( 'NONE', #12951, 5.000000000000004441 ) ;
#1371 = FILL_AREA_STYLE ('',( #7807 ) ) ;
#1372 =( GEOMETRIC_REPRESENTATION_CONTEXT ( 3 ) GLOBAL_UNCERTAINTY_ASSIGNED_CONTEXT ( ( #15779 ) ) GLOBAL_UNIT_ASSIGNED_CONTEXT ( ( #7156, #9093, #4162 ) ) REPRESENTATION_CONTEXT ( 'NONE', 'WORKASPACE' ) );
#1373 = LINE ( 'NONE', #17379, #11528 ) ;
#1374 = EDGE_LOOP ( 'NONE', ( #5976, #16, #6934, #8755 ) ) ;
#1375 = EDGE_CURVE ( 'NONE', #11798, #16010, #10956, .T. ) ;
#1376 = VERTEX_POINT ( 'NONE', #17236 ) ;
#1377 = AXIS2_PLACEMENT_3D ( 'NONE', #19114, #264, #12857 ) ;
#1378 = AXIS2_PLACEMENT_3D ( 'NONE', #9230, #6052, #7499 ) ;
#1379 = ORIENTED_EDGE ( 'NONE', *, *, #13450, .F. ) ;
#1380 = PRODUCT_DEFINITION ( 'UNKNOWN', '', #5359, #8846 ) ;
#1381 = ORIENTED_EDGE ( 'NONE', *, *, #7588, .T. ) ;
#1382 = DIRECTION ( 'NONE',  ( 0.000000000000000000, 0.000000000000000000, 1.000000000000000000 ) ) ;
#1383 = FILL_AREA_STYLE_COLOUR ( '', #3179 ) ;
#1384 = EDGE_LOOP ( 'NONE', ( #4779, #18292, #1588, #8014 ) ) ;
#1385 =( NAMED_UNIT ( * ) PLANE_ANGLE_UNIT ( ) SI_UNIT ( $, .RADIAN. ) );
#1386 = CARTESIAN_POINT ( 'NONE',  ( 10.00000000000000000, 372.8685141053783241, -143.5198051533979537 ) ) ;
#1387 = CLOSED_SHELL ( 'NONE', ( #13518, #808, #12135, #8402, #2091, #17761, #6762, #1836, #15290, #17155, #8765, #538, #17542, #10774, #12423, #12075, #3760, #35, #6916, #3060, #10404, #11440 ) ) ;
#1388 = AXIS2_PLACEMENT_3D ( 'NONE', #17608, #9779, #17190 ) ;
#1389 = ORIENTED_EDGE ( 'NONE', *, *, #1048, .T. ) ;
#1390 = EDGE_CURVE ( 'NONE', #6575, #6561, #3224, .T. ) ;
#1391 = FILL_AREA_STYLE_COLOUR ( '', #8532 ) ;
#1392 = SURFACE_SIDE_STYLE ('',( #9156 ) ) ;
#1393 = DIRECTION ( 'NONE',  ( 1.000000000000000000, 9.815121534730717399E-17, 0.000000000000000000 ) ) ;
#1394 = FACE_OUTER_BOUND ( 'NONE', #17894, .T. ) ;
#1395 = EDGE_CURVE ( 'NONE', #7933, #10796, #14953, .T. ) ;
#1396 = MECHANICAL_DESIGN_GEOMETRIC_PRESENTATION_REPRESENTATION (  '', ( #8668 ), #10314 ) ;
#1397 =( GEOMETRIC_REPRESENTATION_CONTEXT ( 3 ) GLOBAL_UNCERTAINTY_ASSIGNED_CONTEXT ( ( #16729 ) ) GLOBAL_UNIT_ASSIGNED_CONTEXT ( ( #16168, #13080, #8314 ) ) REPRESENTATION_CONTEXT ( 'NONE', 'WORKASPACE' ) );
#1398 = DIRECTION ( 'NONE',  ( -0.000000000000000000, -0.000000000000000000, 1.000000000000000000 ) ) ;
#1399 = CYLINDRICAL_SURFACE ( 'NONE', #972, 4.999999999999997335 ) ;
#1400 = CIRCLE ( 'NONE', #15264, 14.76997474683060041 ) ;
#1401 =( NAMED_UNIT ( * ) PLANE_ANGLE_UNIT ( ) SI_UNIT ( $, .RADIAN. ) );
#1402 = DIRECTION ( 'NONE',  ( -1.000000000000000000, 0.000000000000000000, 0.000000000000000000 ) ) ;
#1403 = APPLICATION_CONTEXT ( 'automotive_design' ) ;
#1404 = EDGE_CURVE ( 'NONE', #5330, #11398, #10849, .T. ) ;
#1405 = VECTOR ( 'NONE', #7683, 1000.000000000000000 ) ;
#1406 = ADVANCED_FACE ( 'NONE', ( #17129 ), #1452, .T. ) ;
#1407 = STYLED_ITEM ( 'NONE', ( #14471 ), #219 ) ;
#1408 = AXIS2_PLACEMENT_3D ( 'NONE', #2410, #948, #7276 ) ;
#1409 = ORIENTED_EDGE ( 'NONE', *, *, #9867, .T. ) ;
#1410 = ORIENTED_EDGE ( 'NONE', *, *, #3355, .T. ) ;
#1411 = EDGE_CURVE ( 'NONE', #13058, #6497, #18882, .T. ) ;
#1412 = ORIENTED_EDGE ( 'NONE', *, *, #12401, .T. ) ;
#1413 = ORIENTED_EDGE ( 'NONE', *, *, #15982, .T. ) ;
#1414 = VECTOR ( 'NONE', #16185, 1000.000000000000000 ) ;
#1415 = STYLED_ITEM ( 'NONE', ( #10441 ), #19301 ) ;
#1416 = ORIENTED_EDGE ( 'NONE', *, *, #9358, .F. ) ;
#1417 = COLOUR_RGB ( '', 0.09019608, 0.27058824, 0.51372549) ;
#1418 = EDGE_CURVE ( 'NONE', #11661, #14090, #14138, .T. ) ;
#1419 = CARTESIAN_POINT ( 'NONE',  ( 40.00000000000001421, 0.000000000000000000, -150.0000000000000000 ) ) ;
#1420 = PRESENTATION_LAYER_ASSIGNMENT (  '', '', ( #1093 ) ) ;
#1421 = DIRECTION ( 'NONE',  ( 1.000000000000000000, -0.000000000000000000, 0.000000000000000000 ) ) ;
#1422 = FILL_AREA_STYLE ('',( #13724 ) ) ;
#1423 =( GEOMETRIC_REPRESENTATION_CONTEXT ( 3 ) GLOBAL_UNCERTAINTY_ASSIGNED_CONTEXT ( ( #13454 ) ) GLOBAL_UNIT_ASSIGNED_CONTEXT ( ( #11249, #2063, #8380 ) ) REPRESENTATION_CONTEXT ( 'NONE', 'WORKASPACE' ) );
#1424 = FACE_OUTER_BOUND ( 'NONE', #6660, .T. ) ;
#1425 = MECHANICAL_DESIGN_GEOMETRIC_PRESENTATION_REPRESENTATION (  '', ( #2429 ), #6064 ) ;
#1426 = CARTESIAN_POINT ( 'NONE',  ( -23.00000000000002132, 10.00000000000000000, 32.00000000000000000 ) ) ;
#1427 = EDGE_CURVE ( 'NONE', #6358, #14517, #1645, .T. ) ;
#1428 =( GEOMETRIC_REPRESENTATION_CONTEXT ( 3 ) GLOBAL_UNCERTAINTY_ASSIGNED_CONTEXT ( ( #10240 ) ) GLOBAL_UNIT_ASSIGNED_CONTEXT ( ( #8408, #3862, #11796 ) ) REPRESENTATION_CONTEXT ( 'NONE', 'WORKASPACE' ) );
#1429 = DIRECTION ( 'NONE',  ( 1.000000000000000000, 0.000000000000000000, -0.000000000000000000 ) ) ;
#1430 = FACE_OUTER_BOUND ( 'NONE', #15415, .T. ) ;
#1431 = ORIENTED_EDGE ( 'NONE', *, *, #16993, .T. ) ;
#1432 = CARTESIAN_POINT ( 'NONE',  ( 17.99999999999998224, 6.000000000000000000, -35.99999999999999289 ) ) ;
#1433 = CARTESIAN_POINT ( 'NONE',  ( -64.99999999999995737, 316.7545334744432353, 495.1946179577816451 ) ) ;
#1434 = VECTOR ( 'NONE', #16449, 1000.000000000000000 ) ;
#1435 = CIRCLE ( 'NONE', #11328, 35.00000000000000711 ) ;
#1436 = VECTOR ( 'NONE', #12800, 1000.000000000000000 ) ;
#1437 = VECTOR ( 'NONE', #17221, 1000.000000000000000 ) ;
#1438 = ADVANCED_FACE ( 'NONE', ( #14244 ), #120, .T. ) ;
#1439 = STYLED_ITEM ( 'NONE', ( #18650 ), #1705 ) ;
#1440 =( GEOMETRIC_REPRESENTATION_CONTEXT ( 3 ) GLOBAL_UNCERTAINTY_ASSIGNED_CONTEXT ( ( #7259 ) ) GLOBAL_UNIT_ASSIGNED_CONTEXT ( ( #6985, #6799, #17791 ) ) REPRESENTATION_CONTEXT ( 'NONE', 'WORKASPACE' ) );
#1441 = ORIENTED_EDGE ( 'NONE', *, *, #17967, .T. ) ;
#1442 = VECTOR ( 'NONE', #14443, 1000.000000000000000 ) ;
#1443 = CARTESIAN_POINT ( 'NONE',  ( 22.99999999999998224, 10.00000000000000000, 37.00000000000000711 ) ) ;
#1444 = VERTEX_POINT ( 'NONE', #6635 ) ;
#1445 = EDGE_CURVE ( 'NONE', #13536, #3873, #6849, .T. ) ;
#1446 = AXIS2_PLACEMENT_3D ( 'NONE', #3134, #13745, #20006 ) ;
#1447 = SURFACE_SIDE_STYLE ('',( #15609 ) ) ;
#1448 = STYLED_ITEM ( 'NONE', ( #18775 ), #19670 ) ;
#1449 = CARTESIAN_POINT ( 'NONE',  ( -81.18192946989275072, 140.4048636633015406, 499.8237260975782874 ) ) ;
#1450 = STYLED_ITEM ( 'NONE', ( #121 ), #15204 ) ;
#1451 = VERTEX_POINT ( 'NONE', #1958 ) ;
#1452 = CYLINDRICAL_SURFACE ( 'NONE', #15626, 8.000000000000000000 ) ;
#1453 = CONICAL_SURFACE ( 'NONE', #14325, 18.17500000000000071, 0.7483780475235185525 ) ;
#1454 = DIRECTION ( 'NONE',  ( 1.000000000000000000, 5.889072920838430686E-16, -0.000000000000000000 ) ) ;
#1455 = EDGE_CURVE ( 'NONE', #19399, #19379, #4978, .T. ) ;
#1456 = CARTESIAN_POINT ( 'NONE',  ( 0.3890055088326604404, 139.8536359628922128, 501.0133158358985384 ) ) ;
#1457 = DIRECTION ( 'NONE',  ( 1.000000000000000000, 0.000000000000000000, 0.000000000000000000 ) ) ;
#1458 = CIRCLE ( 'NONE', #9386, 1.000000000000004219 ) ;
#1459 = SURFACE_SIDE_STYLE ('',( #232 ) ) ;
#1460 = DIRECTION ( 'NONE',  ( -0.000000000000000000, -1.000000000000000000, -0.000000000000000000 ) ) ;
#1461 = CIRCLE ( 'NONE', #11979, 10.00000000000000888 ) ;
#1462 = ORIENTED_EDGE ( 'NONE', *, *, #17441, .T. ) ;
#1463 =( NAMED_UNIT ( * ) SI_UNIT ( $, .STERADIAN. ) SOLID_ANGLE_UNIT ( ) );
#1464 = SHAPE_DEFINITION_REPRESENTATION ( #2002, #7605 ) ;
#1465 = VERTEX_POINT ( 'NONE', #8477 ) ;
#1466 = ORIENTED_EDGE ( 'NONE', *, *, #9563, .F. ) ;
#1467 = DIRECTION ( 'NONE',  ( 0.000000000000000000, -0.000000000000000000, 1.000000000000000000 ) ) ;
#1468 = VERTEX_POINT ( 'NONE', #9716 ) ;
#1469 = VECTOR ( 'NONE', #5943, 1000.000000000000000 ) ;
#1470 = ORIENTED_EDGE ( 'NONE', *, *, #49, .F. ) ;
#1471 = ORIENTED_EDGE ( 'NONE', *, *, #1375, .T. ) ;
#1472 = VECTOR ( 'NONE', #2062, 1000.000000000000000 ) ;
#1473 = ORIENTED_EDGE ( 'NONE', *, *, #10065, .F. ) ;
#1474 = VECTOR ( 'NONE', #12030, 1000.000000000000000 ) ;
#1475 = FILL_AREA_STYLE_COLOUR ( '', #12977 ) ;
#1476 = EDGE_CURVE ( 'NONE', #19519, #15351, #429, .T. ) ;
#1477 = FACE_OUTER_BOUND ( 'NONE', #6236, .T. ) ;
#1478 = CARTESIAN_POINT ( 'NONE',  ( -25.99999999999999645, 68.00000000000000000, -39.99999999999999289 ) ) ;
#1479 = FACE_OUTER_BOUND ( 'NONE', #9785, .T. ) ;
#1480 = SURFACE_SIDE_STYLE ('',( #7889 ) ) ;
#1481 =( NAMED_UNIT ( * ) PLANE_ANGLE_UNIT ( ) SI_UNIT ( $, .RADIAN. ) );
#1482 = VERTEX_POINT ( 'NONE', #10024 ) ;
#1483 = FILL_AREA_STYLE_COLOUR ( '', #11803 ) ;
#1484 = FACE_OUTER_BOUND ( 'NONE', #19692, .T. ) ;
#1485 = CARTESIAN_POINT ( 'NONE',  ( 22.99999999999998224, 10.00000000000000000, -31.00000000000003197 ) ) ;
#1486 = SHAPE_REPRESENTATION_RELATIONSHIP ( 'NONE' , 'NONE' ,  #3934, #2502 ) ;
#1487 =( NAMED_UNIT ( * ) PLANE_ANGLE_UNIT ( ) SI_UNIT ( $, .RADIAN. ) );
#1488 = DIRECTION ( 'NONE',  ( 0.000000000000000000, 0.000000000000000000, -1.000000000000000000 ) ) ;
#1489 = MANIFOLD_SOLID_BREP ( 'Cut-Extrude1', #6378 ) ;
#1490 = CARTESIAN_POINT ( 'NONE',  ( 1.000000000002633005, 139.7703989349544145, 490.5655098179835818 ) ) ;
#1491 = SURFACE_SIDE_STYLE ('',( #14182 ) ) ;
#1492 = ADVANCED_BREP_SHAPE_REPRESENTATION ( '', ( #15383, #15873, #2741 ), #19153 ) ;
#1493 = EDGE_LOOP ( 'NONE', ( #17586, #17289, #5838, #3950 ) ) ;
#1494 = CIRCLE ( 'NONE', #13066, 3.000000000000002665 ) ;
#1495 = VERTEX_POINT ( 'NONE', #8279 ) ;
#1496 = ORIENTED_EDGE ( 'NONE', *, *, #20213, .F. ) ;
#1497 = PRODUCT ( 'din_6885_2_a_6_x_6_x_25', 'din_6885_2_a_6_x_6_x_25', '', ( #10559 ) ) ;
#1498 = ORIENTED_EDGE ( 'NONE', *, *, #20251, .F. ) ;
#1499 = DIRECTION ( 'NONE',  ( 1.000000000000000000, 0.000000000000000000, 0.000000000000000000 ) ) ;
#1500 = ORIENTED_EDGE ( 'NONE', *, *, #3595, .F. ) ;
#1501 = MECHANICAL_DESIGN_GEOMETRIC_PRESENTATION_REPRESENTATION (  '', ( #14036 ), #16371 ) ;
#1502 =( LENGTH_UNIT ( ) NAMED_UNIT ( * ) SI_UNIT ( .MILLI., .METRE. ) );
#1503 = EDGE_CURVE ( 'NONE', #11435, #11592, #8180, .T. ) ;
#1504 =( LENGTH_UNIT ( ) NAMED_UNIT ( * ) SI_UNIT ( .MILLI., .METRE. ) );
#1505 = ORIENTED_EDGE ( 'NONE', *, *, #18314, .T. ) ;
#1506 = AXIS2_PLACEMENT_3D ( 'NONE', #3487, #9769, #16078 ) ;
#1507 = DIRECTION ( 'NONE',  ( 0.000000000000000000, -0.000000000000000000, 1.000000000000000000 ) ) ;
#1508 = DIRECTION ( 'NONE',  ( 0.000000000000000000, 0.000000000000000000, 1.000000000000000000 ) ) ;
#1509 = CARTESIAN_POINT ( 'NONE',  ( -2.601523022692215026, 61.50677485111217635, 9.137549538570182150 ) ) ;
#1510 = CARTESIAN_POINT ( 'NONE',  ( 22.99999999999998224, 10.00000000000000000, -31.00000000000003197 ) ) ;
#1511 = DIRECTION ( 'NONE',  ( 1.000000000000000000, -0.000000000000000000, 0.000000000000000000 ) ) ;
#1512 =( LENGTH_UNIT ( ) NAMED_UNIT ( * ) SI_UNIT ( .MILLI., .METRE. ) );
#1513 = EDGE_CURVE ( 'NONE', #11555, #7705, #18227, .T. ) ;
#1514 = EDGE_LOOP ( 'NONE', ( #16962, #17333, #16515, #11968 ) ) ;
#1515 = ORIENTED_EDGE ( 'NONE', *, *, #9257, .T. ) ;
#1516 = MANIFOLD_SOLID_BREP ( 'Cut-Extrude4[2]', #9986 ) ;
#1517 = VERTEX_POINT ( 'NONE', #6747 ) ;
#1518 = EDGE_LOOP ( 'NONE', ( #17202, #12283, #16460, #635 ) ) ;
#1519 = EDGE_LOOP ( 'NONE', ( #14022, #14032, #2450, #15611 ) ) ;
#1520 = EDGE_LOOP ( 'NONE', ( #17313, #11194, #200, #9789 ) ) ;
#1521 = DIRECTION ( 'NONE',  ( -1.000000000000000000, 0.000000000000000000, -0.000000000000000000 ) ) ;
#1522 = DIRECTION ( 'NONE',  ( 0.000000000000000000, 1.000000000000000000, 0.000000000000000000 ) ) ;
#1523 = DIRECTION ( 'NONE',  ( 3.925231146709346286E-14, -0.7071067811865614505, 0.7071067811865336949 ) ) ;
#1524 = PRESENTATION_STYLE_ASSIGNMENT (( #7743 ) ) ;
#1525 = CARTESIAN_POINT ( 'NONE',  ( 30.99999999999999645, 68.00000000000000000, 31.00000000000001066 ) ) ;
#1526 = SURFACE_STYLE_FILL_AREA ( #9391 ) ;
#1528 = EDGE_CURVE ( 'NONE', #13169, #5210, #17949, .T. ) ;
#1527 = CARTESIAN_POINT ( 'NONE',  ( 36.99999999999999289, 6.000000000000000000, 17.99999999999998934 ) ) ;
#1529 = VECTOR ( 'NONE', #19046, 1000.000000000000000 ) ;
#1530 = CARTESIAN_POINT ( 'NONE',  ( 31.00000000000006395, 0.000000000000000000, -22.99999999999999289 ) ) ;
#1531 =( NAMED_UNIT ( * ) PLANE_ANGLE_UNIT ( ) SI_UNIT ( $, .RADIAN. ) );
#1532 =( NAMED_UNIT ( * ) PLANE_ANGLE_UNIT ( ) SI_UNIT ( $, .RADIAN. ) );
#1533 = SURFACE_STYLE_FILL_AREA ( #1215 ) ;
#1534 = EDGE_CURVE ( 'NONE', #14088, #14515, #326, .T. ) ;
#1535 = ORIENTED_EDGE ( 'NONE', *, *, #9513, .F. ) ;
#1536 = DIRECTION ( 'NONE',  ( 0.000000000000000000, 0.000000000000000000, -1.000000000000000000 ) ) ;
#1537 = EDGE_CURVE ( 'NONE', #19958, #8826, #16425, .T. ) ;
#1538 = COLOUR_RGB ( '', 0.40784314, 0.44705882, 0.49803922) ;
#1539 = ORIENTED_EDGE ( 'NONE', *, *, #2609, .F. ) ;
#1540 = EDGE_CURVE ( 'NONE', #10177, #15780, #7335, .T. ) ;
#1541 = LINE ( 'NONE', #8068, #13840 ) ;
#1542 = ORIENTED_EDGE ( 'NONE', *, *, #14940, .T. ) ;
#1543 = FILL_AREA_STYLE ('',( #11059 ) ) ;
#1544 = DIRECTION ( 'NONE',  ( 1.000000000000000000, 0.000000000000000000, 8.673617379884027583E-16 ) ) ;
#1545 = ORIENTED_EDGE ( 'NONE', *, *, #12654, .T. ) ;
#1546 =( NAMED_UNIT ( * ) SI_UNIT ( $, .STERADIAN. ) SOLID_ANGLE_UNIT ( ) );
#1547 = CARTESIAN_POINT ( 'NONE',  ( -31.00000000000000000, 19.00000000000000000, 30.99999999999999289 ) ) ;
#1549 = EDGE_CURVE ( 'NONE', #20243, #4620, #19584, .T. ) ;
#1548 = DIRECTION ( 'NONE',  ( 0.000000000000000000, 0.000000000000000000, 1.000000000000000000 ) ) ;
#1550 = CARTESIAN_POINT ( 'NONE',  ( 0.8548291518614077322, 139.4861549401841785, 500.2186618924462209 ) ) ;
#1551 = DIRECTION ( 'NONE',  ( -1.000000000000000000, -0.000000000000000000, -0.000000000000000000 ) ) ;
#1552 =( NAMED_UNIT ( * ) SI_UNIT ( $, .STERADIAN. ) SOLID_ANGLE_UNIT ( ) );
#1553 = DIRECTION ( 'NONE',  ( 0.000000000000000000, 0.000000000000000000, 1.000000000000000000 ) ) ;
#1554 = VECTOR ( 'NONE', #19834, 1000.000000000000000 ) ;
#1555 = ORIENTED_EDGE ( 'NONE', *, *, #5833, .T. ) ;
#1556 = CARTESIAN_POINT ( 'NONE',  ( 0.000000000000000000, 372.8685141053783241, -150.1198051533980049 ) ) ;
#1557 = DIRECTION ( 'NONE',  ( 0.000000000000000000, 0.000000000000000000, 1.000000000000000000 ) ) ;
#1558 = FACE_OUTER_BOUND ( 'NONE', #16436, .T. ) ;
#1559 = ITEM_DEFINED_TRANSFORMATION ( 'NONE', 'NONE', #1348,  #2741 ) ;
#1560 = EDGE_CURVE ( 'NONE', #13760, #16530, #13725, .T. ) ;
#1561 = ORIENTED_EDGE ( 'NONE', *, *, #6787, .T. ) ;
#1562 = ORIENTED_EDGE ( 'NONE', *, *, #9631, .F. ) ;
#1563 = EDGE_CURVE ( 'NONE', #7052, #19684, #19987, .T. ) ;
#1564 = ORIENTED_EDGE ( 'NONE', *, *, #15818, .T. ) ;
#1565 = ORIENTED_EDGE ( 'NONE', *, *, #2933, .F. ) ;
#1566 = PLANE ( 'NONE',  #18276 ) ;
#1567 = MECHANICAL_DESIGN_GEOMETRIC_PRESENTATION_REPRESENTATION (  '', ( #7848 ), #4239 ) ;
#1568 = ORIENTED_EDGE ( 'NONE', *, *, #4226, .T. ) ;
#1569 = DIRECTION ( 'NONE',  ( 1.000000000000000000, -0.000000000000000000, 0.000000000000000000 ) ) ;
#1570 = ORIENTED_EDGE ( 'NONE', *, *, #10636, .T. ) ;
#1571 = LINE ( 'NONE', #12431, #5122 ) ;
#1572 =( NAMED_UNIT ( * ) PLANE_ANGLE_UNIT ( ) SI_UNIT ( $, .RADIAN. ) );
#1573 = DIRECTION ( 'NONE',  ( 3.328238341717372086E-14, 0.000000000000000000, -1.000000000000000000 ) ) ;
#1574 = CARTESIAN_POINT ( 'NONE',  ( 88.88953019741013861, 167.9162550801369491, 250.0000000000000000 ) ) ;
#1575 = CARTESIAN_POINT ( 'NONE',  ( -22.00000000000001776, 10.00000000000000000, 33.00000000000000711 ) ) ;
#1576 = DIRECTION ( 'NONE',  ( 0.000000000000000000, 0.000000000000000000, 1.000000000000000000 ) ) ;
#1577 = EDGE_CURVE ( 'NONE', #8466, #183, #15268, .T. ) ;
#1578 = ORIENTED_EDGE ( 'NONE', *, *, #16074, .F. ) ;
#1579 = PRESENTATION_STYLE_ASSIGNMENT (( #19229 ) ) ;
#1580 = DIRECTION ( 'NONE',  ( -1.000000000000000000, -0.000000000000000000, -1.135258727068399668E-15 ) ) ;
#1581 = DIRECTION ( 'NONE',  ( -0.000000000000000000, 0.000000000000000000, -1.000000000000000000 ) ) ;
#1582 = CARTESIAN_POINT ( 'NONE',  ( 32.99999999999998579, 10.00000000000000000, 25.99999999999999645 ) ) ;
#1583 = MANIFOLD_SOLID_BREP ( 'Boss-Extrude2', #14588 ) ;
#1584 = AXIS2_PLACEMENT_3D ( 'NONE', #18046, #2182, #16136 ) ;
#1585 = MECHANICAL_DESIGN_GEOMETRIC_PRESENTATION_REPRESENTATION (  '', ( #3609 ), #3919 ) ;
#1586 = EDGE_CURVE ( 'NONE', #17808, #11049, #16733, .T. ) ;
#1587 = ORIENTED_EDGE ( 'NONE', *, *, #19459, .F. ) ;
#1588 = ORIENTED_EDGE ( 'NONE', *, *, #8262, .F. ) ;
#1589 = ORIENTED_EDGE ( 'NONE', *, *, #8146, .F. ) ;
#1590 = CARTESIAN_POINT ( 'NONE',  ( -79.98592531253316906, 140.1739456240907771, 501.5312821746164218 ) ) ;
#1591 = VERTEX_POINT ( 'NONE', #8677 ) ;
#1592 = AXIS2_PLACEMENT_3D ( 'NONE', #806, #4129, #13412 ) ;
#1593 = CYLINDRICAL_SURFACE ( 'NONE', #11022, 10.00000000000000888 ) ;
#1594 = CIRCLE ( 'NONE', #19033, 1.000000000000000888 ) ;
#1595 = CARTESIAN_POINT ( 'NONE',  ( 1.050000000000000044, -15.25000000000000000, -1.867586368699713770E-15 ) ) ;
#1596 =( GEOMETRIC_REPRESENTATION_CONTEXT ( 3 ) GLOBAL_UNCERTAINTY_ASSIGNED_CONTEXT ( ( #15000 ) ) GLOBAL_UNIT_ASSIGNED_CONTEXT ( ( #16980, #6047, #15331 ) ) REPRESENTATION_CONTEXT ( 'NONE', 'WORKASPACE' ) );
#1597 = ORIENTED_EDGE ( 'NONE', *, *, #1144, .F. ) ;
#1598 = CARTESIAN_POINT ( 'NONE',  ( 503.8334540492693918, 0.000000000000000000, 0.000000000000000000 ) ) ;
#1599 = DIRECTION ( 'NONE',  ( -0.000000000000000000, -0.000000000000000000, -1.000000000000000000 ) ) ;
#1600 = SURFACE_SIDE_STYLE ('',( #1708 ) ) ;
#1601 = EDGE_CURVE ( 'NONE', #19572, #13442, #16636, .T. ) ;
#1602 = SURFACE_STYLE_FILL_AREA ( #2962 ) ;
#1603 = FACE_OUTER_BOUND ( 'NONE', #6979, .T. ) ;
#1604 = FACE_OUTER_BOUND ( 'NONE', #2972, .T. ) ;
#1605 = CARTESIAN_POINT ( 'NONE',  ( 30.99999999999999645, 3.000000000000000000, -25.99999999999999645 ) ) ;
#1606 = FACE_OUTER_BOUND ( 'NONE', #13424, .T. ) ;
#1607 = DIRECTION ( 'NONE',  ( -6.123031769111888756E-17, 1.000000000000000000, 3.749151804555344967E-33 ) ) ;
#1608 = VECTOR ( 'NONE', #11407, 1000.000000000000000 ) ;
#1609 = AXIS2_PLACEMENT_3D ( 'NONE', #6249, #9025, #12119 ) ;
#1610 = CARTESIAN_POINT ( 'NONE',  ( 0.000000000000000000, 0.000000000000000000, 0.000000000000000000 ) ) ;
#1611 = EDGE_CURVE ( 'NONE', #16025, #5632, #4037, .T. ) ;
#1612 = ORIENTED_EDGE ( 'NONE', *, *, #4108, .T. ) ;
#1613 = ORIENTED_EDGE ( 'NONE', *, *, #19709, .F. ) ;
#1614 = ORIENTED_EDGE ( 'NONE', *, *, #9237, .F. ) ;
#1615 = ORIENTED_EDGE ( 'NONE', *, *, #4504, .F. ) ;
#1616 = ORIENTED_EDGE ( 'NONE', *, *, #11550, .T. ) ;
#1617 = CARTESIAN_POINT ( 'NONE',  ( 0.000000000000000000, -3.000000000000000000, 0.000000000000000000 ) ) ;
#1618 = LINE ( 'NONE', #17626, #14274 ) ;
#1619 = FILL_AREA_STYLE ('',( #3202 ) ) ;
#1620 = CIRCLE ( 'NONE', #15157, 4.999999999999997335 ) ;
#1621 = CARTESIAN_POINT ( 'NONE',  ( 108.9893729001365870, 143.5567736071463969, 294.7336993003747239 ) ) ;
#1622 = MECHANICAL_DESIGN_GEOMETRIC_PRESENTATION_REPRESENTATION (  '', ( #11542 ), #14185 ) ;
#1623 =( NAMED_UNIT ( * ) SI_UNIT ( $, .STERADIAN. ) SOLID_ANGLE_UNIT ( ) );
#1624 = DIRECTION ( 'NONE',  ( -0.000000000000000000, 1.000000000000000000, -0.000000000000000000 ) ) ;
#1625 = AXIS2_PLACEMENT_3D ( 'NONE', #7469, #10642, #16840 ) ;
#1626 = CARTESIAN_POINT ( 'NONE',  ( 406.3334540492693350, 242.8734308960556234, 250.0000000000000000 ) ) ;
#1627 = EDGE_CURVE ( 'NONE', #4612, #995, #10672, .T. ) ;
#1628 = LINE ( 'NONE', #12486, #13295 ) ;
#1629 = ORIENTED_EDGE ( 'NONE', *, *, #9788, .F. ) ;
#1630 = CARTESIAN_POINT ( 'NONE',  ( -79.99999999999995737, 152.4824555358011082, 486.3411705753778165 ) ) ;
#1631 = LINE ( 'NONE', #14344, #9700 ) ;
#1632 = VECTOR ( 'NONE', #2614, 1000.000000000000000 ) ;
#1633 = CIRCLE ( 'NONE', #14507, 18.49999999999998934 ) ;
#1634 = VECTOR ( 'NONE', #14358, 1000.000000000000000 ) ;
#1635 = EDGE_CURVE ( 'NONE', #10821, #2527, #3114, .T. ) ;
#1636 = ORIENTED_EDGE ( 'NONE', *, *, #12967, .F. ) ;
#1637 = CARTESIAN_POINT ( 'NONE',  ( 20.99999999999996092, 3.000000000000000000, 35.00000000000000711 ) ) ;
#1638 = ADVANCED_FACE ( 'NONE', ( #8874 ), #6084, .T. ) ;
#1639 = ORIENTED_EDGE ( 'NONE', *, *, #7611, .F. ) ;
#1640 = DIRECTION ( 'NONE',  ( 0.000000000000000000, 0.000000000000000000, -1.000000000000000000 ) ) ;
#1641 = DIRECTION ( 'NONE',  ( 1.000000000000000000, 9.815121534730718631E-17, -0.000000000000000000 ) ) ;
#1642 = EDGE_LOOP ( 'NONE', ( #2207, #13694, #5259, #19708 ) ) ;
#1643 = CARTESIAN_POINT ( 'NONE',  ( -26.00000000000000000, 19.00000000000000000, -31.00000000000003908 ) ) ;
#1644 = MANIFOLD_SOLID_BREP ( 'Boss-Extrude1', #7677 ) ;
#1645 = LINE ( 'NONE', #18869, #5738 ) ;
#1646 = LINE ( 'NONE', #14245, #13340 ) ;
#1647 = AXIS2_PLACEMENT_3D ( 'NONE', #8447, #687, #9981 ) ;
#1648 = CARTESIAN_POINT ( 'NONE',  ( -0.6579963148074815527, 139.9810361770940688, 501.2022436020878899 ) ) ;
#1649 = CIRCLE ( 'NONE', #7936, 14.76997474683060041 ) ;
#1650 = CARTESIAN_POINT ( 'NONE',  ( 0.000000000000000000, -3.000000000000000000, 35.00000000000000711 ) ) ;
#1651 = FACE_OUTER_BOUND ( 'NONE', #17246, .T. ) ;
#1652 = CARTESIAN_POINT ( 'NONE',  ( 0.000000000000000000, 38.00000000000000711, 0.9999999999999943379 ) ) ;
#1653 = EDGE_LOOP ( 'NONE', ( #9323, #1723, #4180, #15193 ) ) ;
#1654 = LINE ( 'NONE', #6440, #1229 ) ;
#1655 = EDGE_CURVE ( 'NONE', #11104, #4860, #20076, .T. ) ;
#1656 = PLANE ( 'NONE',  #11552 ) ;
#1657 = SURFACE_SIDE_STYLE ('',( #13848 ) ) ;
#1658 = ITEM_DEFINED_TRANSFORMATION ( 'NONE', 'NONE', #10275,  #2741 ) ;
#1659 = PRODUCT_DEFINITION_SHAPE ( 'NONE', 'NONE',  #15789 ) ;
#1660 = EDGE_LOOP ( 'NONE', ( #16302, #8956, #4461, #17809 ) ) ;
#1661 = DIRECTION ( 'NONE',  ( 0.000000000000000000, 1.000000000000000000, 0.000000000000000000 ) ) ;
#1662 = ORIENTED_EDGE ( 'NONE', *, *, #5663, .F. ) ;
#1663 = VERTEX_POINT ( 'NONE', #15579 ) ;
#1664 = EDGE_CURVE ( 'NONE', #4662, #19129, #4435, .T. ) ;
#1665 = VERTEX_POINT ( 'NONE', #6197 ) ;
#1666 = COLOUR_RGB ( '', 0.72549020, 0.75294118, 0.79215686) ;
#1667 = CARTESIAN_POINT ( 'NONE',  ( -37.00000000000000000, 68.00000000000000000, 23.00000000000000355 ) ) ;
#1668 = EDGE_CURVE ( 'NONE', #12058, #16534, #7930, .T. ) ;
#1669 = ORIENTED_EDGE ( 'NONE', *, *, #10572, .T. ) ;
#1670 = FILL_AREA_STYLE ('',( #16055 ) ) ;
#1671 = CARTESIAN_POINT ( 'NONE',  ( 7.000000000000000000, 17.68750000000000000, 0.000000000000000000 ) ) ;
#1672 = EDGE_CURVE ( 'NONE', #16358, #9405, #3784, .T. ) ;
#1673 = SURFACE_STYLE_USAGE ( .BOTH. , #18901 ) ;
#1674 = DIRECTION ( 'NONE',  ( 0.000000000000000000, 0.000000000000000000, -1.000000000000000000 ) ) ;
#1675 =( REPRESENTATION_RELATIONSHIP ('NONE','NONE', #13279, #10380 ) REPRESENTATION_RELATIONSHIP_WITH_TRANSFORMATION ( #12730 )SHAPE_REPRESENTATION_RELATIONSHIP( ) );
#1676 = CARTESIAN_POINT ( 'NONE',  ( -80.72548054392764527, 139.7734801347532994, 489.5367579066505073 ) ) ;
#1677 = EDGE_CURVE ( 'NONE', #13170, #17444, #12472, .T. ) ;
#1678 = CYLINDRICAL_SURFACE ( 'NONE', #10364, 36.00000000000000000 ) ;
#1679 = FACE_OUTER_BOUND ( 'NONE', #12164, .T. ) ;
#1680 = DIRECTION ( 'NONE',  ( 8.479266908829339085E-16, -1.000000000000000000, 0.000000000000000000 ) ) ;
#1681 = VERTEX_POINT ( 'NONE', #14020 ) ;
#1682 = EDGE_CURVE ( 'NONE', #8340, #19125, #14211, .T. ) ;
#1683 = DIRECTION ( 'NONE',  ( 0.000000000000000000, -1.000000000000000000, 0.000000000000000000 ) ) ;
#1684 = DIRECTION ( 'NONE',  ( 1.000000000000000000, 9.815121534730717399E-17, -0.000000000000000000 ) ) ;
#1685 = DIRECTION ( 'NONE',  ( -1.000000000000000000, 0.000000000000000000, 0.000000000000000000 ) ) ;
#1686 = CIRCLE ( 'NONE', #8294, 3.299999999999997158 ) ;
#1687 = DIRECTION ( 'NONE',  ( -1.000000000000000000, 0.000000000000000000, 0.000000000000000000 ) ) ;
#1688 = FILL_AREA_STYLE ('',( #3165 ) ) ;
#1689 = LINE ( 'NONE', #2941, #9628 ) ;
#1690 = DIRECTION ( 'NONE',  ( 0.000000000000000000, 0.000000000000000000, 1.000000000000000000 ) ) ;
#1691 = CIRCLE ( 'NONE', #14873, 1.000000000000000888 ) ;
#1692 = DIRECTION ( 'NONE',  ( 1.000000000000000000, -0.000000000000000000, 0.000000000000000000 ) ) ;
#1693 = ORIENTED_EDGE ( 'NONE', *, *, #19168, .T. ) ;
#1694 = CIRCLE ( 'NONE', #15889, 35.00000000000000711 ) ;
#1695 = ORIENTED_EDGE ( 'NONE', *, *, #8362, .F. ) ;
#1696 = VERTEX_POINT ( 'NONE', #4744 ) ;
#1697 = FILL_AREA_STYLE ('',( #18811 ) ) ;
#1698 = MECHANICAL_DESIGN_GEOMETRIC_PRESENTATION_REPRESENTATION (  '', ( #19469 ), #15570 ) ;
#1699 = DIRECTION ( 'NONE',  ( -1.000000000000000000, 0.000000000000000000, 4.956352788505159323E-16 ) ) ;
#1700 = COLOUR_RGB ( '', 0.09019608, 0.27058824, 0.51372549) ;
#1701 = ORIENTED_EDGE ( 'NONE', *, *, #15964, .F. ) ;
#1702 = PRESENTATION_STYLE_ASSIGNMENT (( #4831 ) ) ;
#1703 = PRESENTATION_LAYER_ASSIGNMENT (  '', '', ( #6686 ) ) ;
#1704 = ORIENTED_EDGE ( 'NONE', *, *, #13297, .F. ) ;
#1705 = ADVANCED_FACE ( 'NONE', ( #10612, #13805, #5978 ), #18837, .F. ) ;
#1706 = CARTESIAN_POINT ( 'NONE',  ( 0.000000000000000000, 26.00000000000000000, -36.50000000000000000 ) ) ;
#1707 =( NAMED_UNIT ( * ) SI_UNIT ( $, .STERADIAN. ) SOLID_ANGLE_UNIT ( ) );
#1708 = SURFACE_STYLE_FILL_AREA ( #15769 ) ;
#1709 = ADVANCED_FACE ( 'NONE', ( #17311 ), #9473, .T. ) ;
#1710 = DIRECTION ( 'NONE',  ( 0.000000000000000000, 1.000000000000000000, 0.000000000000000000 ) ) ;
#1711 = VECTOR ( 'NONE', #11232, 1000.000000000000000 ) ;
#1712 = FACE_BOUND ( 'NONE', #8055, .T. ) ;
#1713 = EDGE_CURVE ( 'NONE', #8072, #4150, #8245, .T. ) ;
#1714 = CARTESIAN_POINT ( 'NONE',  ( 25.99999999999997868, 8.000000000000000000, -39.99999999999999289 ) ) ;
#1715 = DIRECTION ( 'NONE',  ( 0.000000000000000000, 0.000000000000000000, -1.000000000000000000 ) ) ;
#1716 = CARTESIAN_POINT ( 'NONE',  ( 53.48937290013659407, 208.2227610943810134, 346.7612763259490407 ) ) ;
#1717 = ORIENTED_EDGE ( 'NONE', *, *, #16071, .T. ) ;
#1718 = DIRECTION ( 'NONE',  ( -1.000000000000000000, 0.000000000000000000, -0.000000000000000000 ) ) ;
#1719 = FACE_OUTER_BOUND ( 'NONE', #956, .T. ) ;
#1720 = PRESENTATION_LAYER_ASSIGNMENT (  '', '', ( #18508 ) ) ;
#1721 = COLOUR_RGB ( '', 0.09019608, 0.27058824, 0.51372549) ;
#1722 = AXIS2_PLACEMENT_3D ( 'NONE', #6869, #13154, #16754 ) ;
#1723 = ORIENTED_EDGE ( 'NONE', *, *, #15034, .T. ) ;
#1724 = EDGE_LOOP ( 'NONE', ( #712, #3861 ) ) ;
#1725 = UNCERTAINTY_MEASURE_WITH_UNIT (LENGTH_MEASURE( 1.000000000000000082E-05 ), #15859, 'distance_accuracy_value', 'NONE');
#1726 = SURFACE_SIDE_STYLE ('',( #3291 ) ) ;
#1727 = ORIENTED_EDGE ( 'NONE', *, *, #14220, .T. ) ;
#1728 = VERTEX_POINT ( 'NONE', #5053 ) ;
#1729 = ORIENTED_EDGE ( 'NONE', *, *, #6370, .F. ) ;
#1730 = CARTESIAN_POINT ( 'NONE',  ( 10.00000000000000000, 309.2289037985890445, -143.5198051533984085 ) ) ;
#1731 = DIRECTION ( 'NONE',  ( 0.000000000000000000, 0.000000000000000000, 1.000000000000000000 ) ) ;
#1732 = LINE ( 'NONE', #19154, #18125 ) ;
#1733 = VECTOR ( 'NONE', #2376, 1000.000000000000000 ) ;
#1734 = CYLINDRICAL_SURFACE ( 'NONE', #19049, 34.00000000000000000 ) ;
#1735 = DIRECTION ( 'NONE',  ( 0.000000000000000000, 0.000000000000000000, -1.000000000000000000 ) ) ;
#1736 = PRESENTATION_STYLE_ASSIGNMENT (( #5 ) ) ;
#1737 = EDGE_CURVE ( 'NONE', #13831, #12278, #8150, .T. ) ;
#1738 = CARTESIAN_POINT ( 'NONE',  ( -40.00000000000000711, 10.00000000000000000, -26.00000000000000000 ) ) ;
#1739 = CARTESIAN_POINT ( 'NONE',  ( -23.00000000000003197, 3.000000000000000000, 34.00000000000000711 ) ) ;
#1740 = CARTESIAN_POINT ( 'NONE',  ( -31.00000000000003197, 3.000000000000000000, -30.99999999999999289 ) ) ;
#1741 = FILL_AREA_STYLE_COLOUR ( '', #7350 ) ;
#1742 = AXIS2_PLACEMENT_3D ( 'NONE', #15046, #4132, #4010 ) ;
#1743 = ORIENTED_EDGE ( 'NONE', *, *, #2449, .F. ) ;
#1744 = CIRCLE ( 'NONE', #12620, 17.85000000000000142 ) ;
#1745 = DIRECTION ( 'NONE',  ( -1.000000000000000000, 0.000000000000000000, 0.000000000000000000 ) ) ;
#1746 = SURFACE_SIDE_STYLE ('',( #18665 ) ) ;
#1747 = VECTOR ( 'NONE', #15870, 1000.000000000000000 ) ;
#1748 = PRESENTATION_LAYER_ASSIGNMENT (  '', '', ( #2074 ) ) ;
#1749 = VECTOR ( 'NONE', #2238, 1000.000000000000000 ) ;
#1750 = ORIENTED_EDGE ( 'NONE', *, *, #9563, .T. ) ;
#1751 = VECTOR ( 'NONE', #12600, 1000.000000000000000 ) ;
#1752 = VERTEX_POINT ( 'NONE', #19034 ) ;
#1753 = FACE_OUTER_BOUND ( 'NONE', #8175, .T. ) ;
#1754 = ORIENTED_EDGE ( 'NONE', *, *, #7794, .F. ) ;
#1755 = AXIS2_PLACEMENT_3D ( 'NONE', #14572, #13064, #16441 ) ;
#1756 = DIRECTION ( 'NONE',  ( 0.000000000000000000, 0.000000000000000000, 1.000000000000000000 ) ) ;
#1757 = SURFACE_SIDE_STYLE ('',( #12923 ) ) ;
#1758 = CYLINDRICAL_SURFACE ( 'NONE', #9054, 1.000000000000015987 ) ;
#1759 = VECTOR ( 'NONE', #3856, 1000.000000000000000 ) ;
#1760 = PRESENTATION_LAYER_ASSIGNMENT (  '', '', ( #2113 ) ) ;
#1761 = CARTESIAN_POINT ( 'NONE',  ( 0.04009716062711748963, 139.6070811926061879, 500.4884095045860590 ) ) ;
#1762 = DIRECTION ( 'NONE',  ( 0.000000000000000000, 7.137148015447440312E-15, -1.000000000000000000 ) ) ;
#1763 = CARTESIAN_POINT ( 'NONE',  ( 1.000000000002633005, 138.7723821175183048, 490.5025619656410640 ) ) ;
#1764 = FACE_OUTER_BOUND ( 'NONE', #9936, .T. ) ;
#1765 = VECTOR ( 'NONE', #13348, 1000.000000000000000 ) ;
#1766 = CARTESIAN_POINT ( 'NONE',  ( 0.000000000000000000, 216.7545334744432921, 515.1946179577817020 ) ) ;
#1767 = ORIENTED_EDGE ( 'NONE', *, *, #8291, .F. ) ;
#1768 = LINE ( 'NONE', #12417, #2588 ) ;
#1769 = DIRECTION ( 'NONE',  ( 0.000000000000000000, 1.000000000000000000, 0.000000000000000000 ) ) ;
#1770 = CARTESIAN_POINT ( 'NONE',  ( -40.00000000000000000, 0.000000000000000000, -25.99999999999999645 ) ) ;
#1771 = APPLICATION_PROTOCOL_DEFINITION ( 'draft international standard', 'automotive_design', 1998, #6316 ) ;
#1772 = VECTOR ( 'NONE', #10430, 1000.000000000000000 ) ;
#1773 = ORIENTED_EDGE ( 'NONE', *, *, #16816, .F. ) ;
#1774 = EDGE_LOOP ( 'NONE', ( #6198, #2231, #6097, #2830 ) ) ;
#1775 = DIRECTION ( 'NONE',  ( 1.000000000000000000, 0.000000000000000000, 3.328238341717372086E-14 ) ) ;
#1776 = VERTEX_POINT ( 'NONE', #17621 ) ;
#1777 = COLOUR_RGB ( '', 0.31764706, 0.68627451, 0.89019608) ;
#1778 = ORIENTED_EDGE ( 'NONE', *, *, #10679, .F. ) ;
#1779 = ORIENTED_EDGE ( 'NONE', *, *, #9646, .T. ) ;
#1780 = EDGE_CURVE ( 'NONE', #3349, #4170, #15304, .T. ) ;
#1781 = COLOUR_RGB ( '', 0.40784314, 0.44705882, 0.49803922) ;
#1782 = CIRCLE ( 'NONE', #142, 2.500000000000002220 ) ;
#1783 = COLOUR_RGB ( '', 0.08235294, 0.09019608, 0.10196078) ;
#1784 = DIRECTION ( 'NONE',  ( 0.000000000000000000, 1.000000000000000000, 0.000000000000000000 ) ) ;
#1785 = FACE_OUTER_BOUND ( 'NONE', #13091, .T. ) ;
#1786 = ORIENTED_EDGE ( 'NONE', *, *, #9186, .F. ) ;
#1787 = CARTESIAN_POINT ( 'NONE',  ( -0.000000000000000000, 80.91625508013694912, 0.000000000000000000 ) ) ;
#1788 = CARTESIAN_POINT ( 'NONE',  ( 34.00000000000002842, 0.000000000000000000, 26.00000000000000355 ) ) ;
#1789 = ORIENTED_EDGE ( 'NONE', *, *, #11501, .F. ) ;
#1790 = DIRECTION ( 'NONE',  ( 0.000000000000000000, 1.000000000000000000, 0.000000000000000000 ) ) ;
#1791 = VECTOR ( 'NONE', #10571, 1000.000000000000000 ) ;
#1792 = LINE ( 'NONE', #18996, #5300 ) ;
#1793 = AXIS2_PLACEMENT_3D ( 'NONE', #4623, #17185, #3065 ) ;
#1794 = CARTESIAN_POINT ( 'NONE',  ( 498.8334540492693918, 167.8734308960555950, 250.0000000000000000 ) ) ;
#1795 = CARTESIAN_POINT ( 'NONE',  ( -31.00000000000003197, 68.00000000000000000, 26.00000000000000355 ) ) ;
#1796 = FACE_OUTER_BOUND ( 'NONE', #19661, .T. ) ;
#1797 = EDGE_CURVE ( 'NONE', #17228, #417, #17521, .T. ) ;
#1798 = CYLINDRICAL_SURFACE ( 'NONE', #1103, 3.000000000000002665 ) ;
#1799 = ORIENTED_EDGE ( 'NONE', *, *, #15038, .F. ) ;
#1800 = FACE_OUTER_BOUND ( 'NONE', #2407, .T. ) ;
#1801 = AXIS2_PLACEMENT_3D ( 'NONE', #6948, #7051, #4164 ) ;
#1802 = DIRECTION ( 'NONE',  ( -0.000000000000000000, -0.000000000000000000, 1.000000000000000000 ) ) ;
#1803 = CARTESIAN_POINT ( 'NONE',  ( -21.00000000000002842, -20.00000000000000000, -37.50000000000000000 ) ) ;
#1804 = LINE ( 'NONE', #15851, #18539 ) ;
#1805 = COLOUR_RGB ( '', 0.08235294, 0.09019608, 0.10196078) ;
#1806 = CARTESIAN_POINT ( 'NONE',  ( 1.181929469893224560, 216.7545334744432921, 499.8237260975781737 ) ) ;
#1807 = AXIS2_PLACEMENT_3D ( 'NONE', #1254, #7585, #13867 ) ;
#1808 = EDGE_CURVE ( 'NONE', #6649, #11502, #6836, .T. ) ;
#1809 = CARTESIAN_POINT ( 'NONE',  ( -0.9575141835544629387, 139.0431362428743682, 488.7923103725937040 ) ) ;
#1810 = PRESENTATION_STYLE_ASSIGNMENT (( #16070 ) ) ;
#1811 = ORIENTED_EDGE ( 'NONE', *, *, #9123, .T. ) ;
#1812 = EDGE_CURVE ( 'NONE', #14622, #11075, #10014, .T. ) ;
#1813 = AXIS2_PLACEMENT_3D ( 'NONE', #18675, #1226, #9194 ) ;
#1814 = DIRECTION ( 'NONE',  ( -0.000000000000000000, -0.000000000000000000, 1.000000000000000000 ) ) ;
#1815 = VECTOR ( 'NONE', #18990, 1000.000000000000000 ) ;
#1816 = ORIENTED_EDGE ( 'NONE', *, *, #4640, .T. ) ;
#1817 = EDGE_CURVE ( 'NONE', #666, #3145, #12693, .T. ) ;
#1818 =( REPRESENTATION_RELATIONSHIP ('NONE','NONE', #12483, #13798 ) REPRESENTATION_RELATIONSHIP_WITH_TRANSFORMATION ( #9205 )SHAPE_REPRESENTATION_RELATIONSHIP( ) );
#1819 = CARTESIAN_POINT ( 'NONE',  ( -80.63015381190217568, 139.7734858225249752, 500.8736181254813573 ) ) ;
#1820 = ORIENTED_EDGE ( 'NONE', *, *, #14720, .T. ) ;
#1821 = LINE ( 'NONE', #20271, #15643 ) ;
#1822 = DIRECTION ( 'NONE',  ( 1.000000000000000000, 9.815121534730718631E-17, -0.000000000000000000 ) ) ;
#1823 = ORIENTED_EDGE ( 'NONE', *, *, #14062, .T. ) ;
#1824 = DIRECTION ( 'NONE',  ( 0.000000000000000000, 0.000000000000000000, 1.000000000000000000 ) ) ;
#1825 = SURFACE_STYLE_USAGE ( .BOTH. , #1600 ) ;
#1826 = EDGE_CURVE ( 'NONE', #19851, #13429, #11455, .T. ) ;
#1827 = CARTESIAN_POINT ( 'NONE',  ( 10.00000000000000000, 309.2289037985890445, -150.1198051533984597 ) ) ;
#1828 = DIRECTION ( 'NONE',  ( 1.000000000000000000, 5.889072920838430686E-16, -0.000000000000000000 ) ) ;
#1829 = AXIS2_PLACEMENT_3D ( 'NONE', #13111, #2028, #15783 ) ;
#1830 = DIRECTION ( 'NONE',  ( -0.000000000000000000, -0.000000000000000000, 1.000000000000000000 ) ) ;
#1831 = DIRECTION ( 'NONE',  ( 0.000000000000000000, 0.000000000000000000, -1.000000000000000000 ) ) ;
#1832 = FILL_AREA_STYLE ('',( #17397 ) ) ;
#1833 = EDGE_LOOP ( 'NONE', ( #12096, #18835 ) ) ;
#1834 = EDGE_CURVE ( 'NONE', #3873, #14347, #3530, .T. ) ;
#1835 = SURFACE_STYLE_FILL_AREA ( #11215 ) ;
#1836 = ADVANCED_FACE ( 'NONE', ( #17832 ), #1857, .T. ) ;
#1837 = VERTEX_POINT ( 'NONE', #14747 ) ;
#1838 = AXIS2_PLACEMENT_3D ( 'NONE', #13789, #20276, #12067 ) ;
#1839 = ORIENTED_EDGE ( 'NONE', *, *, #13826, .F. ) ;
#1840 = ORIENTED_EDGE ( 'NONE', *, *, #15318, .T. ) ;
#1841 = ORIENTED_EDGE ( 'NONE', *, *, #3464, .F. ) ;
#1842 = DIRECTION ( 'NONE',  ( 1.000000000000000000, 1.197852309262419498E-15, -0.000000000000000000 ) ) ;
#1843 =( GEOMETRIC_REPRESENTATION_CONTEXT ( 3 ) GLOBAL_UNCERTAINTY_ASSIGNED_CONTEXT ( ( #17619 ) ) GLOBAL_UNIT_ASSIGNED_CONTEXT ( ( #3816, #2551, #19747 ) ) REPRESENTATION_CONTEXT ( 'NONE', 'WORKASPACE' ) );
#1844 = CARTESIAN_POINT ( 'NONE',  ( -1.301042606982605321E-14, 152.4824555358010798, 501.3921618609452366 ) ) ;
#1845 = CARTESIAN_POINT ( 'NONE',  ( 1.050000000000000044, 0.000000000000000000, 0.000000000000000000 ) ) ;
#1846 = DIRECTION ( 'NONE',  ( -0.000000000000000000, -1.000000000000000000, -0.000000000000000000 ) ) ;
#1847 = DIRECTION ( 'NONE',  ( 0.000000000000000000, 0.000000000000000000, -1.000000000000000000 ) ) ;
#1848 = PRODUCT_DEFINITION_SHAPE ( 'NONE', 'NONE',  #20380 ) ;
#1849 = CARTESIAN_POINT ( 'NONE',  ( 498.8117674897343932, 191.8198460455371333, 81.76606011801540319 ) ) ;
#1850 = SURFACE_STYLE_USAGE ( .BOTH. , #16209 ) ;
#1851 = DIRECTION ( 'NONE',  ( -0.000000000000000000, -1.000000000000000000, -0.000000000000000000 ) ) ;
#1852 = EDGE_CURVE ( 'NONE', #17380, #13927, #1458, .T. ) ;
#1853 = CARTESIAN_POINT ( 'NONE',  ( -82.18192946989277914, 216.7545334744432921, 500.8237260975782874 ) ) ;
#1854 = CARTESIAN_POINT ( 'NONE',  ( -31.00000000000002132, 10.00000000000000000, -31.00000000000000000 ) ) ;
#1855 = AXIS2_PLACEMENT_3D ( 'NONE', #16275, #9963, #7188 ) ;
#1856 = EDGE_LOOP ( 'NONE', ( #6444, #17124, #18690, #18662 ) ) ;
#1857 = CYLINDRICAL_SURFACE ( 'NONE', #18262, 2.000000000000001776 ) ;
#1858 = VERTEX_POINT ( 'NONE', #14540 ) ;
#1859 = ORIENTED_EDGE ( 'NONE', *, *, #3532, .T. ) ;
#1860 = CARTESIAN_POINT ( 'NONE',  ( 423.8334540492694487, 191.8198460455371333, 24.99421986894476078 ) ) ;
#1861 = ORIENTED_EDGE ( 'NONE', *, *, #8741, .F. ) ;
#1862 = PLANE ( 'NONE',  #12048 ) ;
#1863 = DIRECTION ( 'NONE',  ( 0.000000000000000000, 0.000000000000000000, -1.000000000000000000 ) ) ;
#1864 = CARTESIAN_POINT ( 'NONE',  ( -1.000000000000012212, 140.8764026050585301, 502.4686618848270996 ) ) ;
#1865 = CARTESIAN_POINT ( 'NONE',  ( 458.8334540492693350, 191.8198460455371333, 178.2339398819846110 ) ) ;
#1866 = CARTESIAN_POINT ( 'NONE',  ( 25.99999999999999645, 68.00000000000000000, 31.00000000000004619 ) ) ;
#1867 = DIRECTION ( 'NONE',  ( 0.000000000000000000, 0.000000000000000000, -1.000000000000000000 ) ) ;
#1868 = DIRECTION ( 'NONE',  ( 6.123031769111888756E-17, 0.000000000000000000, 1.000000000000000000 ) ) ;
#1869 = VERTEX_POINT ( 'NONE', #615 ) ;
#1870 = FILL_AREA_STYLE ('',( #11159 ) ) ;
#1871 = LINE ( 'NONE', #16617, #19434 ) ;
#1872 = CARTESIAN_POINT ( 'NONE',  ( -31.00000000000005329, 10.00000000000000000, 26.00000000000000000 ) ) ;
#1873 = CONICAL_SURFACE ( 'NONE', #13118, 14.92500000000000071, 1.076854957875310381 ) ;
#1874 = LINE ( 'NONE', #4993, #5993 ) ;
#1875 = ORIENTED_EDGE ( 'NONE', *, *, #9541, .T. ) ;
#1876 = ORIENTED_EDGE ( 'NONE', *, *, #17051, .T. ) ;
#1877 = ADVANCED_FACE ( 'NONE', ( #6518, #16218 ), #2048, .T. ) ;
#1878 = VERTEX_POINT ( 'NONE', #3835 ) ;
#1879 = ORIENTED_EDGE ( 'NONE', *, *, #10634, .T. ) ;
#1880 = ORIENTED_EDGE ( 'NONE', *, *, #467, .T. ) ;
#1881 = VECTOR ( 'NONE', #8183, 1000.000000000000000 ) ;
#1882 = FACE_OUTER_BOUND ( 'NONE', #14799, .T. ) ;
#1883 = DIRECTION ( 'NONE',  ( 0.000000000000000000, 0.000000000000000000, 1.000000000000000000 ) ) ;
#1884 = ORIENTED_EDGE ( 'NONE', *, *, #17957, .F. ) ;
#1885 = DIRECTION ( 'NONE',  ( 0.000000000000000000, 0.000000000000000000, 1.000000000000000000 ) ) ;
#1886 = DIRECTION ( 'NONE',  ( 1.000000000000000000, -0.000000000000000000, 0.000000000000000000 ) ) ;
#1887 = CIRCLE ( 'NONE', #5217, 2.999999999999995559 ) ;
#1888 = CARTESIAN_POINT ( 'NONE',  ( -64.99999999999995737, 317.7545334744432353, 475.1454018718993098 ) ) ;
#1889 = DIRECTION ( 'NONE',  ( 0.000000000000000000, 0.000000000000000000, 1.000000000000000000 ) ) ;
#1890 = FILL_AREA_STYLE_COLOUR ( '', #6584 ) ;
#1891 = DIRECTION ( 'NONE',  ( -0.000000000000000000, 1.000000000000000000, -0.000000000000000000 ) ) ;
#1892 = VERTEX_POINT ( 'NONE', #415 ) ;
#1893 = FACE_OUTER_BOUND ( 'NONE', #11740, .T. ) ;
#1894 = EDGE_CURVE ( 'NONE', #6891, #18687, #8370, .T. ) ;
#1895 = DIRECTION ( 'NONE',  ( -1.000000000000000000, 0.000000000000000000, -1.156482317317870344E-15 ) ) ;
#1896 = CARTESIAN_POINT ( 'NONE',  ( 2.625000000000000000, -14.59999999999999964, -1.787984326755135766E-15 ) ) ;
#1897 = DIRECTION ( 'NONE',  ( 1.000000000000000000, -0.000000000000000000, -0.000000000000000000 ) ) ;
#1898 = ORIENTED_EDGE ( 'NONE', *, *, #1713, .T. ) ;
#1899 = VECTOR ( 'NONE', #17682, 1000.000000000000000 ) ;
#1900 = ORIENTED_EDGE ( 'NONE', *, *, #12305, .F. ) ;
#1901 = EDGE_CURVE ( 'NONE', #6758, #17942, #11703, .T. ) ;
#1902 = VERTEX_POINT ( 'NONE', #7034 ) ;
#1903 = FACE_OUTER_BOUND ( 'NONE', #10130, .T. ) ;
#1904 = CARTESIAN_POINT ( 'NONE',  ( -23.00000000000000000, 68.00000000000000000, -31.00000000000005684 ) ) ;
#1905 = EDGE_LOOP ( 'NONE', ( #1016, #10973, #19641, #10313 ) ) ;
#1906 = EDGE_CURVE ( 'NONE', #7140, #19410, #13350, .T. ) ;
#1907 = ORIENTED_EDGE ( 'NONE', *, *, #5503, .F. ) ;
#1908 = DIRECTION ( 'NONE',  ( 0.000000000000000000, 0.000000000000000000, 1.000000000000000000 ) ) ;
#1909 = FACE_OUTER_BOUND ( 'NONE', #18652, .T. ) ;
#1910 = DIRECTION ( 'NONE',  ( -1.000000000000000000, -0.000000000000000000, -0.000000000000000000 ) ) ;
#1911 = CARTESIAN_POINT ( 'NONE',  ( 1.181929469893224560, 138.7545334744432637, 499.8237260975781737 ) ) ;
#1912 = FACE_OUTER_BOUND ( 'NONE', #5078, .T. ) ;
#1913 =( NAMED_UNIT ( * ) PLANE_ANGLE_UNIT ( ) SI_UNIT ( $, .RADIAN. ) );
#1914 = EDGE_CURVE ( 'NONE', #10863, #19071, #8959, .T. ) ;
#1915 = DIRECTION ( 'NONE',  ( -0.000000000000000000, -1.000000000000000000, 0.000000000000000000 ) ) ;
#1916 = DIRECTION ( 'NONE',  ( 0.000000000000000000, 1.000000000000000000, 0.000000000000000000 ) ) ;
#1917 = CARTESIAN_POINT ( 'NONE',  ( -82.18192946989243808, 139.7703989349477354, 490.5655098180907316 ) ) ;
#1918 = SURFACE_STYLE_FILL_AREA ( #6815 ) ;
#1919 = EDGE_CURVE ( 'NONE', #18726, #8554, #14848, .T. ) ;
#1920 = ORIENTED_EDGE ( 'NONE', *, *, #16701, .T. ) ;
#1921 = EDGE_LOOP ( 'NONE', ( #15017, #9955, #11144, #12425 ) ) ;
#1922 = SHAPE_REPRESENTATION ( 'din_6885_2_a_6_x_6_x_25', ( #2741 ), #7323 ) ;
#1923 = AXIS2_PLACEMENT_3D ( 'NONE', #425, #623, #5191 ) ;
#1924 = ORIENTED_EDGE ( 'NONE', *, *, #12318, .F. ) ;
#1925 = EDGE_CURVE ( 'NONE', #6397, #12344, #19262, .T. ) ;
#1926 = VECTOR ( 'NONE', #8747, 1000.000000000000000 ) ;
#1927 = COLOUR_RGB ( '', 0.08235294, 0.09019608, 0.10196078) ;
#1928 = ORIENTED_EDGE ( 'NONE', *, *, #19444, .F. ) ;
#1929 = DIRECTION ( 'NONE',  ( 1.000000000000000000, 0.000000000000000000, 0.000000000000000000 ) ) ;
#1930 = CARTESIAN_POINT ( 'NONE',  ( 0.000000000000000000, 341.0487089519837696, -133.5000000000032969 ) ) ;
#1931 = CARTESIAN_POINT ( 'NONE',  ( 468.8334540492694487, 214.2156642432025251, 245.0000000000000000 ) ) ;
#1932 = EDGE_CURVE ( 'NONE', #15316, #8829, #18030, .T. ) ;
#1933 = PRESENTATION_STYLE_ASSIGNMENT (( #16107 ) ) ;
#1934 = CARTESIAN_POINT ( 'NONE',  ( 25.99999999999999645, 0.000000000000000000, -39.99999999999999289 ) ) ;
#1935 = EDGE_CURVE ( 'NONE', #867, #548, #4785, .T. ) ;
#1936 = CARTESIAN_POINT ( 'NONE',  ( 40.00000000000000711, 11.00000000000000000, -34.99999999999997868 ) ) ;
#1937 = SURFACE_STYLE_USAGE ( .BOTH. , #11647 ) ;
#1938 = DIRECTION ( 'NONE',  ( -1.000000000000000000, 0.000000000000000000, -0.000000000000000000 ) ) ;
#1939 = AXIS2_PLACEMENT_3D ( 'NONE', #16590, #11840, #13489 ) ;
#1940 = CARTESIAN_POINT ( 'NONE',  ( 0.000000000000000000, 0.000000000000000000, 0.000000000000000000 ) ) ;
#1941 = EDGE_CURVE ( 'NONE', #19071, #18463, #496, .T. ) ;
#1942 = AXIS2_PLACEMENT_3D ( 'NONE', #13206, #16203, #17408 ) ;
#1943 =( NAMED_UNIT ( * ) SI_UNIT ( $, .STERADIAN. ) SOLID_ANGLE_UNIT ( ) );
#1944 = SURFACE_STYLE_FILL_AREA ( #3622 ) ;
#1945 = AXIS2_PLACEMENT_3D ( 'NONE', #8525, #15030, #13579 ) ;
#1946 = EDGE_CURVE ( 'NONE', #3481, #8072, #12029, .T. ) ;
#1947 = LINE ( 'NONE', #11653, #16625 ) ;
#1948 = DIRECTION ( 'NONE',  ( 0.000000000000000000, -1.000000000000000000, 0.000000000000000000 ) ) ;
#1949 = VERTEX_POINT ( 'NONE', #2572 ) ;
#1950 = CARTESIAN_POINT ( 'NONE',  ( 1.181929469893224560, 140.4048636633015406, 499.8237260975782874 ) ) ;
#1951 = ORIENTED_EDGE ( 'NONE', *, *, #8031, .F. ) ;
#1952 =( GEOMETRIC_REPRESENTATION_CONTEXT ( 3 ) GLOBAL_UNCERTAINTY_ASSIGNED_CONTEXT ( ( #14651 ) ) GLOBAL_UNIT_ASSIGNED_CONTEXT ( ( #15966, #11096, #13991 ) ) REPRESENTATION_CONTEXT ( 'NONE', 'WORKASPACE' ) );
#1953 = EDGE_LOOP ( 'NONE', ( #18743, #4944 ) ) ;
#1954 = PLANE ( 'NONE',  #5427 ) ;
#1955 = DIRECTION ( 'NONE',  ( 1.734723475976807094E-15, 0.000000000000000000, -1.000000000000000000 ) ) ;
#1956 = ORIENTED_EDGE ( 'NONE', *, *, #13975, .T. ) ;
#1957 = FACE_OUTER_BOUND ( 'NONE', #12979, .T. ) ;
#1958 = CARTESIAN_POINT ( 'NONE',  ( -26.00000000000002842, 3.000000000000000000, 34.00000000000000711 ) ) ;
#1959 = LINE ( 'NONE', #9820, #11957 ) ;
#1960 = ADVANCED_FACE ( 'NONE', ( #5672, #4240, #5481, #19664, #714 ), #2481, .T. ) ;
#1961 = PRESENTATION_STYLE_ASSIGNMENT (( #3540 ) ) ;
#1962 = DIRECTION ( 'NONE',  ( -0.000000000000000000, -1.000000000000000000, -0.000000000000000000 ) ) ;
#1963 = DIRECTION ( 'NONE',  ( 0.000000000000000000, 0.000000000000000000, -1.000000000000000000 ) ) ;
#1964 = VERTEX_POINT ( 'NONE', #8865 ) ;
#1965 = DIRECTION ( 'NONE',  ( -0.000000000000000000, -1.000000000000000000, -0.000000000000000000 ) ) ;
#1966 = LINE ( 'NONE', #13142, #2659 ) ;
#1967 = SURFACE_SIDE_STYLE ('',( #9931 ) ) ;
#1968 = PRESENTATION_LAYER_ASSIGNMENT (  '', '', ( #11540 ) ) ;
#1969 = EDGE_CURVE ( 'NONE', #10840, #17862, #17940, .T. ) ;
#1970 = COLOUR_RGB ( '', 0.72549020, 0.75294118, 0.79215686) ;
#1971 = AXIS2_PLACEMENT_3D ( 'NONE', #11156, #15511, #1332 ) ;
#1972 = VECTOR ( 'NONE', #7634, 1000.000000000000000 ) ;
#1973 = DIRECTION ( 'NONE',  ( -0.000000000000000000, -0.000000000000000000, 1.000000000000000000 ) ) ;
#1974 = ORIENTED_EDGE ( 'NONE', *, *, #10232, .T. ) ;
#1975 = ORIENTED_EDGE ( 'NONE', *, *, #11903, .T. ) ;
#1976 = ORIENTED_EDGE ( 'NONE', *, *, #17810, .F. ) ;
#1977 = CARTESIAN_POINT ( 'NONE',  ( 5.425003271131650706, 0.000000000000000000, 0.000000000000000000 ) ) ;
#1978 = ORIENTED_EDGE ( 'NONE', *, *, #12942, .F. ) ;
#1979 = DIRECTION ( 'NONE',  ( 0.000000000000000000, 1.000000000000000000, 0.000000000000000000 ) ) ;
#1980 = VECTOR ( 'NONE', #16805, 1000.000000000000000 ) ;
#1981 = CARTESIAN_POINT ( 'NONE',  ( 3.000000000000000000, 41.00000000000000711, 9.013878188659973034 ) ) ;
#1982 = EDGE_LOOP ( 'NONE', ( #11263, #10070, #7892, #18376 ) ) ;
#1983 = AXIS2_PLACEMENT_3D ( 'NONE', #20160, #11082, #3248 ) ;
#1984 = FILL_AREA_STYLE_COLOUR ( '', #10984 ) ;
#1985 = CARTESIAN_POINT ( 'NONE',  ( 78.48937290013661539, 80.91625508013694912, 250.0000000000000000 ) ) ;
#1986 = SURFACE_STYLE_FILL_AREA ( #15166 ) ;
#1987 = PLANE ( 'NONE',  #10703 ) ;
#1988 =( NAMED_UNIT ( * ) SI_UNIT ( $, .STERADIAN. ) SOLID_ANGLE_UNIT ( ) );
#1989 = ADVANCED_FACE ( 'NONE', ( #15210 ), #16865, .F. ) ;
#1990 = LINE ( 'NONE', #19317, #19238 ) ;
#1991 = ORIENTED_EDGE ( 'NONE', *, *, #6654, .T. ) ;
#1992 = DIRECTION ( 'NONE',  ( -1.000000000000000000, -0.000000000000000000, -0.000000000000000000 ) ) ;
#1993 = DIRECTION ( 'NONE',  ( 1.000000000000000000, -0.000000000000000000, 0.000000000000000000 ) ) ;
#1994 = PRESENTATION_STYLE_ASSIGNMENT (( #11595 ) ) ;
#1995 = PRESENTATION_STYLE_ASSIGNMENT (( #11496 ) ) ;
#1996 = DIRECTION ( 'NONE',  ( 0.000000000000000000, 0.000000000000000000, 1.000000000000000000 ) ) ;
#1997 = FACE_OUTER_BOUND ( 'NONE', #316, .T. ) ;
#1998 = CARTESIAN_POINT ( 'NONE',  ( 25.99999999999997513, 10.00000000000000000, 31.00000000000003553 ) ) ;
#1999 = VECTOR ( 'NONE', #10175, 1000.000000000000000 ) ;
#2000 = CIRCLE ( 'NONE', #6962, 17.52499999999999858 ) ;
#2001 = VERTEX_POINT ( 'NONE', #1055 ) ;
#2002 = PRODUCT_DEFINITION_SHAPE ( 'NONE', 'NONE',  #2914 ) ;
#2003 = ORIENTED_EDGE ( 'NONE', *, *, #13776, .T. ) ;
#2004 = DIRECTION ( 'NONE',  ( 0.000000000000000000, 0.000000000000000000, -1.000000000000000000 ) ) ;
#2005 = CARTESIAN_POINT ( 'NONE',  ( -79.69598282171878623, 139.7376548800553167, 500.7557224526424307 ) ) ;
#2006 = EDGE_LOOP ( 'NONE', ( #15847, #2250, #6200, #269 ) ) ;
#2007 = CARTESIAN_POINT ( 'NONE',  ( -37.00000000000000711, 10.00000000000000000, 23.00000000000000000 ) ) ;
#2008 = ORIENTED_EDGE ( 'NONE', *, *, #19260, .F. ) ;
#2009 = CARTESIAN_POINT ( 'NONE',  ( 31.00000000000002842, 68.00000000000000000, 23.00000000000001066 ) ) ;
#2010 = AXIS2_PLACEMENT_3D ( 'NONE', #17468, #14181, #4705 ) ;
#2011 = DIRECTION ( 'NONE',  ( 1.000000000000000000, 0.000000000000000000, 0.000000000000000000 ) ) ;
#2012 =( LENGTH_UNIT ( ) NAMED_UNIT ( * ) SI_UNIT ( .MILLI., .METRE. ) );
#2013 = CARTESIAN_POINT ( 'NONE',  ( -81.18192946989275072, 138.7545334744432637, 499.8237260975782874 ) ) ;
#2014 = DIRECTION ( 'NONE',  ( 0.000000000000000000, 1.000000000000000000, 0.000000000000000000 ) ) ;
#2015 = DIRECTION ( 'NONE',  ( 0.000000000000000000, 0.000000000000000000, 1.000000000000000000 ) ) ;
#2016 = EDGE_CURVE ( 'NONE', #11845, #5865, #11686, .T. ) ;
#2017 = CARTESIAN_POINT ( 'NONE',  ( 78.48937290013660117, 123.1299228374914208, 170.4174721992565082 ) ) ;
#2018 = ORIENTED_EDGE ( 'NONE', *, *, #16709, .T. ) ;
#2019 = DIRECTION ( 'NONE',  ( 1.000000000000000000, -0.000000000000000000, -0.000000000000000000 ) ) ;
#2020 = CARTESIAN_POINT ( 'NONE',  ( -211.5106270998635409, 103.1299228374912360, 170.4174721992565082 ) ) ;
#2021 = ORIENTED_EDGE ( 'NONE', *, *, #17080, .F. ) ;
#2022 = VERTEX_POINT ( 'NONE', #10179 ) ;
#2023 = VECTOR ( 'NONE', #12615, 1000.000000000000000 ) ;
#2024 = ORIENTED_EDGE ( 'NONE', *, *, #15402, .F. ) ;
#2025 = ORIENTED_EDGE ( 'NONE', *, *, #6622, .F. ) ;
#2026 = ORIENTED_EDGE ( 'NONE', *, *, #18842, .T. ) ;
#2027 = EDGE_CURVE ( 'NONE', #183, #5483, #19741, .T. ) ;
#2028 = DIRECTION ( 'NONE',  ( -0.000000000000000000, -1.000000000000000000, -0.000000000000000000 ) ) ;
#2029 = CARTESIAN_POINT ( 'NONE',  ( 463.8334540492693350, 214.2156642432025251, 250.0000000000000000 ) ) ;
#2030 = AXIS2_PLACEMENT_3D ( 'NONE', #10574, #10675, #16978 ) ;
#2031 = LINE ( 'NONE', #19649, #6148 ) ;
#2032 = LINE ( 'NONE', #14638, #106 ) ;
#2033 = CARTESIAN_POINT ( 'NONE',  ( 1.836909530733565148E-16, 0.000000000000000000, 3.000000000000000000 ) ) ;
#2034 = PLANE ( 'NONE',  #6507 ) ;
#2035 = AXIS2_PLACEMENT_3D ( 'NONE', #19137, #3501, #2015 ) ;
#2036 = VECTOR ( 'NONE', #9134, 1000.000000000000000 ) ;
#2037 = PLANE ( 'NONE',  #19550 ) ;
#2038 = EDGE_CURVE ( 'NONE', #13405, #14242, #11939, .T. ) ;
#2039 = FILL_AREA_STYLE_COLOUR ( '', #2970 ) ;
#2040 = EDGE_CURVE ( 'NONE', #11158, #11636, #4131, .T. ) ;
#2041 = CARTESIAN_POINT ( 'NONE',  ( 1.181929469892510243, 139.7703989349544145, 489.5655098179833544 ) ) ;
#2042 = DIRECTION ( 'NONE',  ( 1.000000000000000000, -0.000000000000000000, -0.000000000000000000 ) ) ;
#2043 = SURFACE_SIDE_STYLE ('',( #6500 ) ) ;
#2044 = COLOUR_RGB ( '', 0.08235294, 0.09019608, 0.10196078) ;
#2045 = EDGE_CURVE ( 'NONE', #3236, #7608, #4215, .T. ) ;
#2046 = EDGE_CURVE ( 'NONE', #18003, #503, #12760, .T. ) ;
#2047 = ORIENTED_EDGE ( 'NONE', *, *, #14318, .T. ) ;
#2048 = PLANE ( 'NONE',  #18582 ) ;
#2049 = UNCERTAINTY_MEASURE_WITH_UNIT (LENGTH_MEASURE( 1.000000000000000082E-05 ), #5162, 'distance_accuracy_value', 'NONE');
#2050 = EDGE_LOOP ( 'NONE', ( #3191, #20110, #17646, #14843 ) ) ;
#2051 = AXIS2_PLACEMENT_3D ( 'NONE', #17748, #2174, #8478 ) ;
#2052 = AXIS2_PLACEMENT_3D ( 'NONE', #17164, #1580, #20350 ) ;
#2053 = EDGE_CURVE ( 'NONE', #16598, #9315, #9648, .T. ) ;
#2054 = AXIS2_PLACEMENT_3D ( 'NONE', #7912, #6377, #15765 ) ;
#2055 = CARTESIAN_POINT ( 'NONE',  ( 18.99999999999998224, 8.000000000000000000, -39.99999999999999289 ) ) ;
#2056 = EDGE_LOOP ( 'NONE', ( #10422, #7508, #11914, #799 ) ) ;
#2057 = ADVANCED_FACE ( 'NONE', ( #8121 ), #2275, .T. ) ;
#2058 = UNCERTAINTY_MEASURE_WITH_UNIT (LENGTH_MEASURE( 1.000000000000000082E-05 ), #8285, 'distance_accuracy_value', 'NONE');
#2059 = FACE_OUTER_BOUND ( 'NONE', #11379, .T. ) ;
#2060 = UNCERTAINTY_MEASURE_WITH_UNIT (LENGTH_MEASURE( 1.000000000000000082E-05 ), #15267, 'distance_accuracy_value', 'NONE');
#2061 = ORIENTED_EDGE ( 'NONE', *, *, #757, .F. ) ;
#2062 = DIRECTION ( 'NONE',  ( -0.000000000000000000, -1.000000000000000000, -0.000000000000000000 ) ) ;
#2063 =( NAMED_UNIT ( * ) PLANE_ANGLE_UNIT ( ) SI_UNIT ( $, .RADIAN. ) );
#2064 = DIRECTION ( 'NONE',  ( 0.000000000000000000, 0.000000000000000000, -1.000000000000000000 ) ) ;
#2065 = CLOSED_SHELL ( 'NONE', ( #3585, #13041, #2334, #5565, #16861, #8508, #7526 ) ) ;
#2066 = AXIS2_PLACEMENT_3D ( 'NONE', #20280, #1285, #8947 ) ;
#2067 = CARTESIAN_POINT ( 'NONE',  ( -31.00000000000002842, 68.00000000000000000, -25.99999999999999645 ) ) ;
#2068 = CARTESIAN_POINT ( 'NONE',  ( 423.8334540492694487, 191.8198460455371333, 158.2339398819845826 ) ) ;
#2069 = EDGE_CURVE ( 'NONE', #15261, #13635, #13044, .T. ) ;
#2070 = ORIENTED_EDGE ( 'NONE', *, *, #1455, .T. ) ;
#2071 = CARTESIAN_POINT ( 'NONE',  ( 133.4893729001365443, 113.1299228374914634, 170.4174721992565082 ) ) ;
#2072 = DIRECTION ( 'NONE',  ( -0.000000000000000000, 1.000000000000000000, -0.000000000000000000 ) ) ;
#2073 = CIRCLE ( 'NONE', #17225, 10.00000000000000888 ) ;
#2074 = STYLED_ITEM ( 'NONE', ( #1995 ), #18833 ) ;
#2075 = SURFACE_STYLE_USAGE ( .BOTH. , #1967 ) ;
#2076 = CONTEXT_DEPENDENT_SHAPE_REPRESENTATION ( #17888, #13850 ) ;
#2077 = DIRECTION ( 'NONE',  ( -3.854941057726250916E-16, 0.000000000000000000, -1.000000000000000000 ) ) ;
#2078 = APPLICATION_CONTEXT ( 'automotive_design' ) ;
#2079 = ORIENTED_EDGE ( 'NONE', *, *, #16300, .T. ) ;
#2080 = VECTOR ( 'NONE', #12265, 1000.000000000000000 ) ;
#2081 = EDGE_LOOP ( 'NONE', ( #20014, #11456, #17037, #4517 ) ) ;
#2082 = EDGE_CURVE ( 'NONE', #3644, #6446, #11711, .T. ) ;
#2083 = ORIENTED_EDGE ( 'NONE', *, *, #5096, .T. ) ;
#2084 = CIRCLE ( 'NONE', #12999, 8.000000000000000000 ) ;
#2085 = DIRECTION ( 'NONE',  ( 0.000000000000000000, 1.000000000000000000, 0.000000000000000000 ) ) ;
#2086 = ORIENTED_EDGE ( 'NONE', *, *, #12382, .T. ) ;
#2087 = UNCERTAINTY_MEASURE_WITH_UNIT (LENGTH_MEASURE( 1.000000000000000082E-05 ), #20169, 'distance_accuracy_value', 'NONE');
#2088 = VECTOR ( 'NONE', #6691, 1000.000000000000000 ) ;
#2089 = PLANE ( 'NONE',  #17912 ) ;
#2090 = VECTOR ( 'NONE', #10357, 1000.000000000000000 ) ;
#2091 = ADVANCED_FACE ( 'NONE', ( #753 ), #12408, .T. ) ;
#2092 = CARTESIAN_POINT ( 'NONE',  ( 108.9893729001365870, 143.7407018517681649, 294.8816803532602080 ) ) ;
#2093 = PRESENTATION_LAYER_ASSIGNMENT (  '', '', ( #17291 ) ) ;
#2094 = VERTEX_POINT ( 'NONE', #16842 ) ;
#2095 = VECTOR ( 'NONE', #7347, 1000.000000000000000 ) ;
#2096 = DIRECTION ( 'NONE',  ( -1.000000000000000000, 0.000000000000000000, 0.000000000000000000 ) ) ;
#2097 = LINE ( 'NONE', #6872, #15669 ) ;
#2098 =( LENGTH_UNIT ( ) NAMED_UNIT ( * ) SI_UNIT ( .MILLI., .METRE. ) );
#2099 = CARTESIAN_POINT ( 'NONE',  ( 40.00000000000001421, 0.000000000000000000, -150.0000000000000000 ) ) ;
#2100 = COLOUR_RGB ( '', 0.31764706, 0.68627451, 0.89019608) ;
#2101 = ORIENTED_EDGE ( 'NONE', *, *, #6169, .T. ) ;
#2102 = DIRECTION ( 'NONE',  ( 0.000000000000000000, -0.000000000000000000, -1.000000000000000000 ) ) ;
#2103 = CARTESIAN_POINT ( 'NONE',  ( 53.48937290013658696, 113.1299228374914065, 170.4174721992565082 ) ) ;
#2104 = DIRECTION ( 'NONE',  ( 0.000000000000000000, -0.000000000000000000, -1.000000000000000000 ) ) ;
#2105 = FILL_AREA_STYLE_COLOUR ( '', #6039 ) ;
#2106 = DIRECTION ( 'NONE',  ( 0.000000000000000000, 0.000000000000000000, 1.000000000000000000 ) ) ;
#2107 = ORIENTED_EDGE ( 'NONE', *, *, #5273, .T. ) ;
#2108 = DIRECTION ( 'NONE',  ( -0.000000000000000000, -0.000000000000000000, 1.000000000000000000 ) ) ;
#2109 = EDGE_CURVE ( 'NONE', #9451, #9045, #9108, .T. ) ;
#2110 = FILL_AREA_STYLE ('',( #17579 ) ) ;
#2111 = VERTEX_POINT ( 'NONE', #4267 ) ;
#2112 = VECTOR ( 'NONE', #8465, 1000.000000000000000 ) ;
#2113 = STYLED_ITEM ( 'NONE', ( #10547 ), #15136 ) ;
#2114 = AXIS2_PLACEMENT_3D ( 'NONE', #6728, #10200, #18025 ) ;
#2115 = VERTEX_POINT ( 'NONE', #1136 ) ;
#2116 = AXIS2_PLACEMENT_3D ( 'NONE', #10322, #5799, #7150 ) ;
#2117 = EDGE_LOOP ( 'NONE', ( #7011, #20203, #11383, #9350, #2366, #4082, #11985, #287, #933, #14652, #16890, #8101, #15522, #12348, #1272, #5792 ) ) ;
#2118 = CARTESIAN_POINT ( 'NONE',  ( 423.8334540492694487, 191.8198460455371333, 24.99421986894476078 ) ) ;
#2119 = CARTESIAN_POINT ( 'NONE',  ( 31.00000000000000711, 0.000000000000000000, -30.99999999999999289 ) ) ;
#2120 = VECTOR ( 'NONE', #11148, 1000.000000000000000 ) ;
#2121 = ORIENTED_EDGE ( 'NONE', *, *, #11033, .F. ) ;
#2122 = DIRECTION ( 'NONE',  ( -0.000000000000000000, -1.000000000000000000, -0.000000000000000000 ) ) ;
#2123 = FILL_AREA_STYLE ('',( #17697 ) ) ;
#2124 = ORIENTED_EDGE ( 'NONE', *, *, #3129, .T. ) ;
#2125 = AXIS2_PLACEMENT_3D ( 'NONE', #17346, #18978, #1868 ) ;
#2126 = FACE_OUTER_BOUND ( 'NONE', #9690, .T. ) ;
#2127 = STYLED_ITEM ( 'NONE', ( #9038 ), #15379 ) ;
#2128 = CARTESIAN_POINT ( 'NONE',  ( 133.4893729001365443, 103.1299228374914492, 79.58252780074349175 ) ) ;
#2129 = CARTESIAN_POINT ( 'NONE',  ( -0.6025106023757541562, 138.8732404265368814, 489.6068043582602627 ) ) ;
#2130 = AXIS2_PLACEMENT_3D ( 'NONE', #11707, #5514, #16159 ) ;
#2131 = LINE ( 'NONE', #375, #12985 ) ;
#2132 = CYLINDRICAL_SURFACE ( 'NONE', #4228, 10.00000000000000178 ) ;
#2133 = FACE_OUTER_BOUND ( 'NONE', #18239, .T. ) ;
#2134 = FACE_BOUND ( 'NONE', #17596, .T. ) ;
#2135 = VECTOR ( 'NONE', #8552, 1000.000000000000000 ) ;
#2136 =( NAMED_UNIT ( * ) SI_UNIT ( $, .STERADIAN. ) SOLID_ANGLE_UNIT ( ) );
#2137 = VECTOR ( 'NONE', #12955, 1000.000000000000000 ) ;
#2138 = FACE_OUTER_BOUND ( 'NONE', #12205, .T. ) ;
#2139 = PRESENTATION_STYLE_ASSIGNMENT (( #19140 ) ) ;
#2140 = VERTEX_POINT ( 'NONE', #7472 ) ;
#2141 = CIRCLE ( 'NONE', #18905, 2.999999999999999556 ) ;
#2142 = ORIENTED_EDGE ( 'NONE', *, *, #7255, .F. ) ;
#2143 = VERTEX_POINT ( 'NONE', #7558 ) ;
#2144 = CIRCLE ( 'NONE', #1090, 1.000000000000000888 ) ;
#2145 = EDGE_CURVE ( 'NONE', #19958, #469, #16970, .T. ) ;
#2146 = ORIENTED_EDGE ( 'NONE', *, *, #19640, .T. ) ;
#2147 = ORIENTED_EDGE ( 'NONE', *, *, #11417, .F. ) ;
#2148 = DIRECTION ( 'NONE',  ( -0.000000000000000000, -1.000000000000000000, -0.000000000000000000 ) ) ;
#2149 = CIRCLE ( 'NONE', #8078, 3.000000000000016431 ) ;
#2150 = CARTESIAN_POINT ( 'NONE',  ( 40.00000000000001421, 0.000000000000000000, 0.000000000000000000 ) ) ;
#2151 = DIRECTION ( 'NONE',  ( -0.000000000000000000, 1.000000000000000000, -0.000000000000000000 ) ) ;
#2152 = CARTESIAN_POINT ( 'NONE',  ( 110.6609457753903882, 211.0574367717017594, 346.4752554294134939 ) ) ;
#2153 = CARTESIAN_POINT ( 'NONE',  ( -40.00000000000000711, 10.00000000000000000, -19.00000000000000355 ) ) ;
#2154 = CARTESIAN_POINT ( 'NONE',  ( 1.163414457778310218E-15, 63.00000000000000000, 9.500000000000000000 ) ) ;
#2155 = CARTESIAN_POINT ( 'NONE',  ( 178.4893729001365443, 145.9162550801369491, 250.0000000000000000 ) ) ;
#2156 = FACE_OUTER_BOUND ( 'NONE', #1050, .T. ) ;
#2157 = CARTESIAN_POINT ( 'NONE',  ( 463.8334540492693350, 191.8198460455371333, 168.2339398819845826 ) ) ;
#2158 = EDGE_CURVE ( 'NONE', #9243, #16969, #2149, .T. ) ;
#2159 = CARTESIAN_POINT ( 'NONE',  ( -79.99999999999995737, 316.7545334744432353, 515.1946179577817020 ) ) ;
#2160 = CIRCLE ( 'NONE', #848, 3.000000000000000000 ) ;
#2161 = VERTEX_POINT ( 'NONE', #18575 ) ;
#2162 =( LENGTH_UNIT ( ) NAMED_UNIT ( * ) SI_UNIT ( .MILLI., .METRE. ) );
#2163 = ORIENTED_EDGE ( 'NONE', *, *, #10165, .T. ) ;
#2164 = EDGE_LOOP ( 'NONE', ( #3428, #16999, #16164, #20184 ) ) ;
#2165 = VERTEX_POINT ( 'NONE', #18770 ) ;
#2166 = EDGE_CURVE ( 'NONE', #19208, #4579, #2902, .T. ) ;
#2167 = CARTESIAN_POINT ( 'NONE',  ( 153.4893729001366864, 113.1299228374914634, 79.58252780074349175 ) ) ;
#2168 = LINE ( 'NONE', #11562, #13633 ) ;
#2169 = CARTESIAN_POINT ( 'NONE',  ( 88.88953019741013861, 167.9162550801369491, 245.0000000000000000 ) ) ;
#2170 = ORIENTED_EDGE ( 'NONE', *, *, #16469, .F. ) ;
#2171 =( NAMED_UNIT ( * ) PLANE_ANGLE_UNIT ( ) SI_UNIT ( $, .RADIAN. ) );
#2172 = PRESENTATION_STYLE_ASSIGNMENT (( #11364 ) ) ;
#2173 = AXIS2_PLACEMENT_3D ( 'NONE', #16496, #11541, #4130 ) ;
#2174 = DIRECTION ( 'NONE',  ( 0.000000000000000000, -0.7071067811865336949, 0.7071067811865614505 ) ) ;
#2175 = EDGE_CURVE ( 'NONE', #20182, #11766, #5911, .T. ) ;
#2176 = VECTOR ( 'NONE', #6405, 1000.000000000000000 ) ;
#2177 = CARTESIAN_POINT ( 'NONE',  ( 53.48937290013659407, 127.7247684487574304, 252.0000000000000000 ) ) ;
#2178 = PRESENTATION_STYLE_ASSIGNMENT (( #10029 ) ) ;
#2179 = DIRECTION ( 'NONE',  ( 1.000000000000000000, 5.889072920838430686E-16, -0.000000000000000000 ) ) ;
#2180 = CARTESIAN_POINT ( 'NONE',  ( -39.99999999999999289, 0.000000000000000000, 34.99999999999997868 ) ) ;
#2181 = ORIENTED_EDGE ( 'NONE', *, *, #5155, .F. ) ;
#2182 = DIRECTION ( 'NONE',  ( -0.000000000000000000, -1.000000000000000000, 0.000000000000000000 ) ) ;
#2183 = CARTESIAN_POINT ( 'NONE',  ( 498.8117674897343932, 191.8198460455371333, 14.99421986894475012 ) ) ;
#2184 = EDGE_CURVE ( 'NONE', #9454, #10177, #4360, .T. ) ;
#2185 = EDGE_CURVE ( 'NONE', #17444, #16566, #8428, .T. ) ;
#2186 = ORIENTED_EDGE ( 'NONE', *, *, #4845, .T. ) ;
#2187 = ORIENTED_EDGE ( 'NONE', *, *, #9612, .T. ) ;
#2188 = LINE ( 'NONE', #7328, #7773 ) ;
#2189 = EDGE_CURVE ( 'NONE', #13471, #4146, #16660, .T. ) ;
#2190 = ORIENTED_EDGE ( 'NONE', *, *, #9848, .T. ) ;
#2191 = FILL_AREA_STYLE ('',( #8491 ) ) ;
#2192 = CARTESIAN_POINT ( 'NONE',  ( 0.7808854937525596673, 38.09666348058623697, 9.469847369592788056 ) ) ;
#2193 = ORIENTED_EDGE ( 'NONE', *, *, #13762, .T. ) ;
#2194 = DIRECTION ( 'NONE',  ( 0.000000000000000000, 0.000000000000000000, 1.000000000000000000 ) ) ;
#2195 = CARTESIAN_POINT ( 'NONE',  ( 493.8117674897343363, 214.2156642432025251, 250.0000000000000000 ) ) ;
#2196 = DIRECTION ( 'NONE',  ( -0.000000000000000000, -1.000000000000000000, -0.000000000000000000 ) ) ;
#2197 = DIRECTION ( 'NONE',  ( 1.000000000000000000, 5.889072920838430686E-16, -0.000000000000000000 ) ) ;
#2198 = ADVANCED_FACE ( 'NONE', ( #9299 ), #13942, .T. ) ;
#2199 = CARTESIAN_POINT ( 'NONE',  ( -2.979937318121947509, 40.60126023706489917, 9.020623939867236984 ) ) ;
#2200 = VECTOR ( 'NONE', #19756, 1000.000000000000000 ) ;
#2201 = ORIENTED_EDGE ( 'NONE', *, *, #6920, .F. ) ;
#2202 =( LENGTH_UNIT ( ) NAMED_UNIT ( * ) SI_UNIT ( .MILLI., .METRE. ) );
#2203 = FILL_AREA_STYLE_COLOUR ( '', #14563 ) ;
#2204 = CARTESIAN_POINT ( 'NONE',  ( 0.000000000000000000, 0.000000000000000000, 250.0000000000000000 ) ) ;
#2205 =( NAMED_UNIT ( * ) PLANE_ANGLE_UNIT ( ) SI_UNIT ( $, .RADIAN. ) );
#2206 = SURFACE_STYLE_FILL_AREA ( #17881 ) ;
#2207 = ORIENTED_EDGE ( 'NONE', *, *, #7625, .F. ) ;
#2208 = ORIENTED_EDGE ( 'NONE', *, *, #12498, .F. ) ;
#2209 = MANIFOLD_SOLID_BREP ( 'Imported1', #8660 ) ;
#2210 = CIRCLE ( 'NONE', #4540, 10.00000000000000888 ) ;
#2211 = AXIS2_PLACEMENT_3D ( 'NONE', #3801, #17899, #10271 ) ;
#2212 = ORIENTED_EDGE ( 'NONE', *, *, #3838, .F. ) ;
#2213 = ORIENTED_EDGE ( 'NONE', *, *, #11649, .F. ) ;
#2214 = SURFACE_STYLE_FILL_AREA ( #3486 ) ;
#2215 = CARTESIAN_POINT ( 'NONE',  ( 78.48937290013660117, 113.1299228374914208, 29.36128450348865471 ) ) ;
#2216 = VERTEX_POINT ( 'NONE', #9593 ) ;
#2217 = EDGE_CURVE ( 'NONE', #17253, #19266, #15504, .T. ) ;
#2218 = ORIENTED_EDGE ( 'NONE', *, *, #13696, .T. ) ;
#2219 = FILL_AREA_STYLE_COLOUR ( '', #9882 ) ;
#2220 = FACE_OUTER_BOUND ( 'NONE', #11476, .T. ) ;
#2221 = CARTESIAN_POINT ( 'NONE',  ( 0.02255891082085830293, 139.0238496639661037, 488.8482061044569491 ) ) ;
#2222 = CARTESIAN_POINT ( 'NONE',  ( -31.00000000000000000, 19.00000000000000000, 30.99999999999999289 ) ) ;
#2223 = EDGE_CURVE ( 'NONE', #10797, #3197, #16228, .T. ) ;
#2224 = LINE ( 'NONE', #8523, #20220 ) ;
#2225 = CARTESIAN_POINT ( 'NONE',  ( -211.5106270998635409, 113.1299228374912502, 170.4174721992565082 ) ) ;
#2226 = PLANE ( 'NONE',  #1945 ) ;
#2227 = VECTOR ( 'NONE', #19937, 1000.000000000000000 ) ;
#2228 = ORIENTED_EDGE ( 'NONE', *, *, #9900, .F. ) ;
#2229 =( NAMED_UNIT ( * ) PLANE_ANGLE_UNIT ( ) SI_UNIT ( $, .RADIAN. ) );
#2230 = EDGE_LOOP ( 'NONE', ( #2624, #7326 ) ) ;
#2231 = ORIENTED_EDGE ( 'NONE', *, *, #3266, .T. ) ;
#2232 = ORIENTED_EDGE ( 'NONE', *, *, #14175, .F. ) ;
#2233 = ORIENTED_EDGE ( 'NONE', *, *, #16026, .T. ) ;
#2234 = ORIENTED_EDGE ( 'NONE', *, *, #13196, .F. ) ;
#2235 = CARTESIAN_POINT ( 'NONE',  ( -78.99999999999997158, 139.1621397082989233, 488.3874972750760435 ) ) ;
#2236 = LINE ( 'NONE', #11637, #18885 ) ;
#2237 = CARTESIAN_POINT ( 'NONE',  ( -79.99999999999995737, 138.7545334744432637, 478.3411705753777596 ) ) ;
#2238 = DIRECTION ( 'NONE',  ( -1.000000000000000000, -0.000000000000000000, -0.000000000000000000 ) ) ;
#2239 = DIRECTION ( 'NONE',  ( 0.000000000000000000, 0.000000000000000000, -1.000000000000000000 ) ) ;
#2240 = FILL_AREA_STYLE_COLOUR ( '', #7739 ) ;
#2241 = CARTESIAN_POINT ( 'NONE',  ( -36.00000000000000711, 10.00000000000000000, -18.00000000000000355 ) ) ;
#2242 = FACE_BOUND ( 'NONE', #4408, .T. ) ;
#2243 = CARTESIAN_POINT ( 'NONE',  ( 0.000000000000000000, 316.7545334744432921, 205.1946179577815883 ) ) ;
#2244 = CARTESIAN_POINT ( 'NONE',  ( -3.000000000000000000, 41.00000000000000711, 6.000000000000000000 ) ) ;
#2245 = CARTESIAN_POINT ( 'NONE',  ( 31.99999999999998579, 6.000000000000000000, 25.99999999999999645 ) ) ;
#2246 = EDGE_CURVE ( 'NONE', #4537, #867, #11363, .T. ) ;
#2247 = DIRECTION ( 'NONE',  ( 0.000000000000000000, 0.000000000000000000, 1.000000000000000000 ) ) ;
#2248 = CARTESIAN_POINT ( 'NONE',  ( -26.00000000000000000, 19.00000000000000000, -40.00000000000000711 ) ) ;
#2249 = CIRCLE ( 'NONE', #5256, 10.00000000000000888 ) ;
#2250 = ORIENTED_EDGE ( 'NONE', *, *, #7475, .T. ) ;
#2251 = ORIENTED_EDGE ( 'NONE', *, *, #15471, .T. ) ;
#2252 = DIRECTION ( 'NONE',  ( 1.000000000000000000, 1.197852309262419498E-15, -0.000000000000000000 ) ) ;
#2253 = UNCERTAINTY_MEASURE_WITH_UNIT (LENGTH_MEASURE( 1.000000000000000082E-05 ), #1235, 'distance_accuracy_value', 'NONE');
#2254 = ORIENTED_EDGE ( 'NONE', *, *, #9130, .F. ) ;
#2255 = ORIENTED_EDGE ( 'NONE', *, *, #9807, .T. ) ;
#2256 = ORIENTED_EDGE ( 'NONE', *, *, #923, .T. ) ;
#2257 = UNCERTAINTY_MEASURE_WITH_UNIT (LENGTH_MEASURE( 1.000000000000000082E-05 ), #17186, 'distance_accuracy_value', 'NONE');
#2258 = LINE ( 'NONE', #13225, #7908 ) ;
#2259 = MECHANICAL_DESIGN_GEOMETRIC_PRESENTATION_REPRESENTATION (  '', ( #20025 ), #2930 ) ;
#2260 = VERTEX_POINT ( 'NONE', #17745 ) ;
#2261 = ADVANCED_FACE ( 'NONE', ( #1957 ), #13038, .F. ) ;
#2262 = DIRECTION ( 'NONE',  ( -9.815121534730717399E-17, 1.000000000000000000, 0.000000000000000000 ) ) ;
#2263 =( GEOMETRIC_REPRESENTATION_CONTEXT ( 3 ) GLOBAL_UNCERTAINTY_ASSIGNED_CONTEXT ( ( #7108 ) ) GLOBAL_UNIT_ASSIGNED_CONTEXT ( ( #13008, #11442, #13114 ) ) REPRESENTATION_CONTEXT ( 'NONE', 'WORKASPACE' ) );
#2264 = CARTESIAN_POINT ( 'NONE',  ( -33.00000000000000000, 8.000000000000000000, -26.00000000000000355 ) ) ;
#2265 = AXIS2_PLACEMENT_3D ( 'NONE', #12224, #15436, #1265 ) ;
#2266 = CARTESIAN_POINT ( 'NONE',  ( 40.00000000000003553, 0.000000000000000000, 26.00000000000000355 ) ) ;
#2267 = FACE_OUTER_BOUND ( 'NONE', #7036, .T. ) ;
#2268 = CARTESIAN_POINT ( 'NONE',  ( -26.00000000000000355, 19.00000000000000000, 31.00000000000003197 ) ) ;
#2269 = ORIENTED_EDGE ( 'NONE', *, *, #11172, .F. ) ;
#2270 = DIRECTION ( 'NONE',  ( -0.000000000000000000, -1.000000000000000000, -1.632680918566406547E-16 ) ) ;
#2271 = LINE ( 'NONE', #2500, #6735 ) ;
#2272 = PRESENTATION_STYLE_ASSIGNMENT (( #2075 ) ) ;
#2273 = CONTEXT_DEPENDENT_SHAPE_REPRESENTATION ( #20104, #6648 ) ;
#2274 = ADVANCED_FACE ( 'NONE', ( #14354 ), #3433, .F. ) ;
#2275 = PLANE ( 'NONE',  #7439 ) ;
#2276 = VECTOR ( 'NONE', #16885, 1000.000000000000000 ) ;
#2277 = AXIS2_PLACEMENT_3D ( 'NONE', #19428, #5336, #10077 ) ;
#2278 = AXIS2_PLACEMENT_3D ( 'NONE', #15184, #13640, #19905 ) ;
#2279 = PRODUCT_RELATED_PRODUCT_CATEGORY ( 'part', '', ( #18958 ) ) ;
#2280 = EDGE_LOOP ( 'NONE', ( #14129, #18966, #10486, #19919, #6519 ) ) ;
#2281 = ORIENTED_EDGE ( 'NONE', *, *, #9691, .F. ) ;
#2282 = ORIENTED_EDGE ( 'NONE', *, *, #14155, .T. ) ;
#2283 = EDGE_CURVE ( 'NONE', #12201, #9147, #14662, .T. ) ;
#2284 = CARTESIAN_POINT ( 'NONE',  ( 178.4893729001365443, 145.9162550801369491, -97.94896630388704750 ) ) ;
#2285 = CARTESIAN_POINT ( 'NONE',  ( 2.383743612111322463, 39.16804506571254763, 9.196765735797566066 ) ) ;
#2286 = UNCERTAINTY_MEASURE_WITH_UNIT (LENGTH_MEASURE( 1.000000000000000082E-05 ), #1502, 'distance_accuracy_value', 'NONE');
#2287 = VERTEX_POINT ( 'NONE', #11151 ) ;
#2288 = DIRECTION ( 'NONE',  ( -1.000000000000000000, 0.000000000000000000, -3.854941057726246479E-16 ) ) ;
#2289 =( NAMED_UNIT ( * ) SI_UNIT ( $, .STERADIAN. ) SOLID_ANGLE_UNIT ( ) );
#2290 = DIRECTION ( 'NONE',  ( 0.000000000000000000, 1.000000000000000000, 0.000000000000000000 ) ) ;
#2291 = EDGE_CURVE ( 'NONE', #8271, #16331, #14243, .T. ) ;
#2292 = PRESENTATION_LAYER_ASSIGNMENT (  '', '', ( #16173 ) ) ;
#2293 = CARTESIAN_POINT ( 'NONE',  ( 31.00000000000001421, 0.000000000000000000, 22.99999999999999645 ) ) ;
#2294 = VECTOR ( 'NONE', #19645, 1000.000000000000000 ) ;
#2295 = AXIS2_PLACEMENT_3D ( 'NONE', #2468, #15920, #3542 ) ;
#2296 = STYLED_ITEM ( 'NONE', ( #7043 ), #6214 ) ;
#2297 = DIRECTION ( 'NONE',  ( 1.000000000000000000, 0.000000000000000000, 0.000000000000000000 ) ) ;
#2298 = ORIENTED_EDGE ( 'NONE', *, *, #2803, .T. ) ;
#2299 = CARTESIAN_POINT ( 'NONE',  ( 53.48937290013659407, 211.0574367717017594, 346.4752554294135507 ) ) ;
#2300 = DIRECTION ( 'NONE',  ( 0.000000000000000000, 1.000000000000000000, 0.000000000000000000 ) ) ;
#2301 = DIRECTION ( 'NONE',  ( 0.000000000000000000, 1.632680918566406793E-16, -1.000000000000000000 ) ) ;
#2302 = CARTESIAN_POINT ( 'NONE',  ( 53.48937290013658696, 113.1299228374914065, 220.6387154965113382 ) ) ;
#2303 = FACE_OUTER_BOUND ( 'NONE', #14795, .T. ) ;
#2304 =( NAMED_UNIT ( * ) SI_UNIT ( $, .STERADIAN. ) SOLID_ANGLE_UNIT ( ) );
#2305 = EDGE_CURVE ( 'NONE', #6700, #10453, #19184, .T. ) ;
#2306 = ORIENTED_EDGE ( 'NONE', *, *, #17461, .F. ) ;
#2307 = CARTESIAN_POINT ( 'NONE',  ( 0.000000000000000000, 0.000000000000000000, 245.0000000000000000 ) ) ;
#2308 = EDGE_LOOP ( 'NONE', ( #3245, #7438, #18335, #7044 ) ) ;
#2309 = ORIENTED_EDGE ( 'NONE', *, *, #950, .F. ) ;
#2310 = EDGE_CURVE ( 'NONE', #13659, #17347, #534, .T. ) ;
#2311 = ORIENTED_EDGE ( 'NONE', *, *, #8965, .F. ) ;
#2312 = EDGE_CURVE ( 'NONE', #9509, #3967, #18971, .T. ) ;
#2313 = ORIENTED_EDGE ( 'NONE', *, *, #12617, .T. ) ;
#2314 = EDGE_LOOP ( 'NONE', ( #5407, #10763, #2974, #1539, #14422, #16401, #5352, #4326 ) ) ;
#2315 = DIRECTION ( 'NONE',  ( 0.000000000000000000, -1.000000000000000000, 0.000000000000000000 ) ) ;
#2316 = DIRECTION ( 'NONE',  ( 0.000000000000000000, 0.000000000000000000, -1.000000000000000000 ) ) ;
#2317 = ORIENTED_EDGE ( 'NONE', *, *, #7836, .T. ) ;
#2318 = EDGE_CURVE ( 'NONE', #2111, #13550, #19072, .T. ) ;
#2319 = CYLINDRICAL_SURFACE ( 'NONE', #19561, 18.49999999999998934 ) ;
#2320 =( LENGTH_UNIT ( ) NAMED_UNIT ( * ) SI_UNIT ( .MILLI., .METRE. ) );
#2321 = VECTOR ( 'NONE', #3722, 1000.000000000000114 ) ;
#2322 = EDGE_CURVE ( 'NONE', #5003, #17127, #16031, .T. ) ;
#2323 = FACE_OUTER_BOUND ( 'NONE', #10236, .T. ) ;
#2324 = FACE_OUTER_BOUND ( 'NONE', #16415, .T. ) ;
#2325 = CARTESIAN_POINT ( 'NONE',  ( 0.8686015887051632411, 139.7703989352353346, 489.5655098179837523 ) ) ;
#2326 = DIRECTION ( 'NONE',  ( 2.125007447556912624E-15, -0.7817866094812263578, -0.6235460666509320404 ) ) ;
#2327 = DIRECTION ( 'NONE',  ( 0.000000000000000000, 0.000000000000000000, -1.000000000000000000 ) ) ;
#2328 = PRESENTATION_LAYER_ASSIGNMENT (  '', '', ( #5961 ) ) ;
#2329 = AXIS2_PLACEMENT_3D ( 'NONE', #18828, #8029, #12781 ) ;
#2330 = FILL_AREA_STYLE ('',( #18400 ) ) ;
#2331 = AXIS2_PLACEMENT_3D ( 'NONE', #16731, #15586, #18655 ) ;
#2332 = DIRECTION ( 'NONE',  ( 0.000000000000000000, 0.000000000000000000, 1.000000000000000000 ) ) ;
#2333 = FACE_OUTER_BOUND ( 'NONE', #10143, .T. ) ;
#2334 = ADVANCED_FACE ( 'NONE', ( #3319 ), #1862, .F. ) ;
#2335 = UNCERTAINTY_MEASURE_WITH_UNIT (LENGTH_MEASURE( 1.000000000000000082E-05 ), #7424, 'distance_accuracy_value', 'NONE');
#2336 = CARTESIAN_POINT ( 'NONE',  ( 423.8334540492694487, 191.8198460455371333, 168.2339398819845826 ) ) ;
#2337 = ORIENTED_EDGE ( 'NONE', *, *, #17605, .F. ) ;
#2338 = ORIENTED_EDGE ( 'NONE', *, *, #4510, .F. ) ;
#2339 = ORIENTED_EDGE ( 'NONE', *, *, #7763, .T. ) ;
#2340 = ORIENTED_EDGE ( 'NONE', *, *, #11790, .F. ) ;
#2341 = VERTEX_POINT ( 'NONE', #5085 ) ;
#2342 = EDGE_CURVE ( 'NONE', #7513, #9045, #14549, .T. ) ;
#2343 =( LENGTH_UNIT ( ) NAMED_UNIT ( * ) SI_UNIT ( .MILLI., .METRE. ) );
#2344 = AXIS2_PLACEMENT_3D ( 'NONE', #16458, #13082, #14589 ) ;
#2345 = DIRECTION ( 'NONE',  ( 0.000000000000000000, 1.000000000000000000, 0.000000000000000000 ) ) ;
#2346 = FACE_OUTER_BOUND ( 'NONE', #4948, .T. ) ;
#2347 = ADVANCED_FACE ( 'NONE', ( #9819, #11062, #16128, #428, #6746 ), #19294, .F. ) ;
#2348 = FACE_BOUND ( 'NONE', #7928, .T. ) ;
#2349 = VECTOR ( 'NONE', #12868, 1000.000000000000000 ) ;
#2350 = FACE_OUTER_BOUND ( 'NONE', #8991, .T. ) ;
#2351 = EDGE_CURVE ( 'NONE', #17151, #7933, #10023, .T. ) ;
#2352 = CYLINDRICAL_SURFACE ( 'NONE', #2173, 1.000000000000000888 ) ;
#2353 = CARTESIAN_POINT ( 'NONE',  ( 178.4893729001365443, 145.9162550801369491, 250.0000000000000000 ) ) ;
#2354 = LINE ( 'NONE', #17068, #14251 ) ;
#2355 = CARTESIAN_POINT ( 'NONE',  ( 0.9999999999998859801, 140.4048636633015406, 500.8237260975781737 ) ) ;
#2356 = CYLINDRICAL_SURFACE ( 'NONE', #6033, 10.00000000000000888 ) ;
#2357 = DIRECTION ( 'NONE',  ( 1.000000000000000000, -0.000000000000000000, -0.000000000000000000 ) ) ;
#2358 = CARTESIAN_POINT ( 'NONE',  ( -77.99033078109007988, 127.7247684487574304, 357.7985149490353933 ) ) ;
#2359 =( NAMED_UNIT ( * ) PLANE_ANGLE_UNIT ( ) SI_UNIT ( $, .RADIAN. ) );
#2360 = AXIS2_PLACEMENT_3D ( 'NONE', #18287, #16669, #20013 ) ;
#2361 = PRESENTATION_LAYER_ASSIGNMENT (  '', '', ( #71 ) ) ;
#2362 = VERTEX_POINT ( 'NONE', #16635 ) ;
#2363 = EDGE_LOOP ( 'NONE', ( #17108, #13667, #16054, #4191 ) ) ;
#2364 = VECTOR ( 'NONE', #8519, 1000.000000000000000 ) ;
#2365 = DIRECTION ( 'NONE',  ( -0.000000000000000000, -1.000000000000000000, 0.000000000000000000 ) ) ;
#2366 = ORIENTED_EDGE ( 'NONE', *, *, #2803, .F. ) ;
#2367 = ORIENTED_EDGE ( 'NONE', *, *, #4353, .T. ) ;
#2368 = ORIENTED_EDGE ( 'NONE', *, *, #308, .F. ) ;
#2369 = EDGE_CURVE ( 'NONE', #12704, #12426, #14755, .T. ) ;
#2370 = CARTESIAN_POINT ( 'NONE',  ( 18.99999999999998224, 8.000000000000000000, -39.99999999999999289 ) ) ;
#2371 = VECTOR ( 'NONE', #18001, 1000.000000000000000 ) ;
#2372 = VECTOR ( 'NONE', #5639, 1000.000000000000000 ) ;
#2373 =( NAMED_UNIT ( * ) SI_UNIT ( $, .STERADIAN. ) SOLID_ANGLE_UNIT ( ) );
#2374 = EDGE_LOOP ( 'NONE', ( #9766, #15777, #1639, #9611 ) ) ;
#2375 = CARTESIAN_POINT ( 'NONE',  ( -82.18192946989240966, 138.7545334744432637, 489.5655098179820470 ) ) ;
#2376 = DIRECTION ( 'NONE',  ( -1.000000000000000000, -0.000000000000000000, 1.017652531801993019E-13 ) ) ;
#2377 = PRESENTATION_LAYER_ASSIGNMENT (  '', '', ( #8974 ) ) ;
#2378 = CARTESIAN_POINT ( 'NONE',  ( 53.48937290013659407, 167.9162550801369491, -97.94896630388704750 ) ) ;
#2379 = CARTESIAN_POINT ( 'NONE',  ( -25.99999999999999645, 0.000000000000000000, -39.99999999999999289 ) ) ;
#2380 = DIRECTION ( 'NONE',  ( 1.000000000000000000, 0.000000000000000000, 0.000000000000000000 ) ) ;
#2381 = MECHANICAL_DESIGN_GEOMETRIC_PRESENTATION_REPRESENTATION (  '', ( #9974 ), #17517 ) ;
#2382 = ORIENTED_EDGE ( 'NONE', *, *, #10228, .T. ) ;
#2383 = DIRECTION ( 'NONE',  ( 1.000000000000000000, -0.000000000000000000, 0.000000000000000000 ) ) ;
#2384 = DIRECTION ( 'NONE',  ( -0.000000000000000000, -1.000000000000000000, -0.000000000000000000 ) ) ;
#2385 = CARTESIAN_POINT ( 'NONE',  ( 31.00000000000003553, 8.000000000000000000, 20.99999999999999289 ) ) ;
#2386 = DIRECTION ( 'NONE',  ( 1.000000000000000000, 1.197852309262419498E-15, -0.000000000000000000 ) ) ;
#2387 = AXIS2_PLACEMENT_3D ( 'NONE', #15853, #17278, #17377 ) ;
#2388 = VECTOR ( 'NONE', #13121, 1000.000000000000000 ) ;
#2389 = ORIENTED_EDGE ( 'NONE', *, *, #14416, .T. ) ;
#2390 = ORIENTED_EDGE ( 'NONE', *, *, #3879, .F. ) ;
#2391 = EDGE_CURVE ( 'NONE', #2478, #2627, #15067, .T. ) ;
#2392 = STYLED_ITEM ( 'NONE', ( #1736 ), #35 ) ;
#2393 = ORIENTED_EDGE ( 'NONE', *, *, #5814, .F. ) ;
#2394 = FACE_BOUND ( 'NONE', #5528, .T. ) ;
#2395 = FACE_BOUND ( 'NONE', #17737, .T. ) ;
#2396 = ORIENTED_EDGE ( 'NONE', *, *, #17549, .F. ) ;
#2397 = CARTESIAN_POINT ( 'NONE',  ( -34.99999999999998579, -20.00000000000000000, 21.00000000000000355 ) ) ;
#2398 = CARTESIAN_POINT ( 'NONE',  ( -79.31189707736970718, 140.0116299656163505, 501.2541794163659574 ) ) ;
#2399 =( NAMED_UNIT ( * ) SI_UNIT ( $, .STERADIAN. ) SOLID_ANGLE_UNIT ( ) );
#2400 = FILL_AREA_STYLE_COLOUR ( '', #10666 ) ;
#2401 = AXIS2_PLACEMENT_3D ( 'NONE', #6412, #7746, #12699 ) ;
#2402 = VECTOR ( 'NONE', #7999, 1000.000000000000000 ) ;
#2403 = UNCERTAINTY_MEASURE_WITH_UNIT (LENGTH_MEASURE( 1.000000000000000082E-05 ), #3894, 'distance_accuracy_value', 'NONE');
#2404 = FACE_OUTER_BOUND ( 'NONE', #1774, .T. ) ;
#2405 = SURFACE_STYLE_USAGE ( .BOTH. , #13249 ) ;
#2406 = FILL_AREA_STYLE_COLOUR ( '', #8038 ) ;
#2407 = EDGE_LOOP ( 'NONE', ( #19427, #12874, #9683, #19289 ) ) ;
#2408 = DIRECTION ( 'NONE',  ( 0.000000000000000000, 0.000000000000000000, 1.000000000000000000 ) ) ;
#2409 = CARTESIAN_POINT ( 'NONE',  ( -44.50085094405407915, 159.0821755739672483, 510.3921618609452935 ) ) ;
#2410 = CARTESIAN_POINT ( 'NONE',  ( 94.48937290013506640, 117.9618363720963714, 579.5438326823516491 ) ) ;
#2411 = AXIS2_PLACEMENT_3D ( 'NONE', #15062, #3557, #17554 ) ;
#2412 = FILL_AREA_STYLE_COLOUR ( '', #387 ) ;
#2413 =( GEOMETRIC_REPRESENTATION_CONTEXT ( 3 ) GLOBAL_UNCERTAINTY_ASSIGNED_CONTEXT ( ( #2650 ) ) GLOBAL_UNIT_ASSIGNED_CONTEXT ( ( #6675, #14587, #17984 ) ) REPRESENTATION_CONTEXT ( 'NONE', 'WORKASPACE' ) );
#2414 = EDGE_CURVE ( 'NONE', #3980, #15201, #11720, .T. ) ;
#2415 = ORIENTED_EDGE ( 'NONE', *, *, #13797, .F. ) ;
#2416 = ORIENTED_EDGE ( 'NONE', *, *, #15113, .F. ) ;
#2417 = VERTEX_POINT ( 'NONE', #626 ) ;
#2418 = VECTOR ( 'NONE', #12729, 1000.000000000000000 ) ;
#2419 = VECTOR ( 'NONE', #10101, 1000.000000000000000 ) ;
#2420 = AXIS2_PLACEMENT_3D ( 'NONE', #19592, #6855, #7161 ) ;
#2421 = ORIENTED_EDGE ( 'NONE', *, *, #3726, .T. ) ;
#2422 = ORIENTED_EDGE ( 'NONE', *, *, #7753, .T. ) ;
#2423 = CARTESIAN_POINT ( 'NONE',  ( 53.48937290013659407, 127.7247684487574304, 252.0000000000000000 ) ) ;
#2424 = DIRECTION ( 'NONE',  ( 0.000000000000000000, 1.000000000000000000, 0.000000000000000000 ) ) ;
#2425 = VERTEX_POINT ( 'NONE', #14971 ) ;
#2426 = VECTOR ( 'NONE', #6943, 1000.000000000000000 ) ;
#2427 = EDGE_CURVE ( 'NONE', #8147, #14816, #2799, .T. ) ;
#2428 = SURFACE_STYLE_USAGE ( .BOTH. , #1060 ) ;
#2429 = STYLED_ITEM ( 'NONE', ( #3515 ), #418 ) ;
#2430 = LINE ( 'NONE', #16385, #13815 ) ;
#2431 = CARTESIAN_POINT ( 'NONE',  ( 0.000000000000000000, 5.000000000000000888, 0.000000000000000000 ) ) ;
#2432 = CARTESIAN_POINT ( 'NONE',  ( 0.7188359785814644187, 138.8395712689028301, 489.5362691342353401 ) ) ;
#2433 = FILL_AREA_STYLE_COLOUR ( '', #7715 ) ;
#2434 = EDGE_CURVE ( 'NONE', #6152, #2022, #14019, .T. ) ;
#2435 = DIRECTION ( 'NONE',  ( 0.000000000000000000, 0.000000000000000000, 1.000000000000000000 ) ) ;
#2436 = MECHANICAL_DESIGN_GEOMETRIC_PRESENTATION_REPRESENTATION (  '', ( #16304 ), #9360 ) ;
#2437 = PRESENTATION_LAYER_ASSIGNMENT (  '', '', ( #2773 ) ) ;
#2438 = DIRECTION ( 'NONE',  ( -0.000000000000000000, -1.000000000000000000, -0.000000000000000000 ) ) ;
#2439 = DIRECTION ( 'NONE',  ( 0.000000000000000000, 0.000000000000000000, -1.000000000000000000 ) ) ;
#2440 = FACE_BOUND ( 'NONE', #7812, .T. ) ;
#2441 = PRESENTATION_LAYER_ASSIGNMENT (  '', '', ( #7403 ) ) ;
#2442 = DIRECTION ( 'NONE',  ( 1.141265444721583757E-16, -1.000000000000000000, 0.000000000000000000 ) ) ;
#2443 = FILL_AREA_STYLE_COLOUR ( '', #15541 ) ;
#2444 = DIRECTION ( 'NONE',  ( -0.000000000000000000, -0.000000000000000000, -1.000000000000000000 ) ) ;
#2445 = ORIENTED_EDGE ( 'NONE', *, *, #18313, .F. ) ;
#2446 = ADVANCED_FACE ( 'NONE', ( #19669 ), #18620, .T. ) ;
#2447 = VECTOR ( 'NONE', #16824, 1000.000000000000000 ) ;
#2448 = VECTOR ( 'NONE', #3586, 1000.000000000000000 ) ;
#2449 = EDGE_CURVE ( 'NONE', #4636, #4060, #3843, .T. ) ;
#2450 = ORIENTED_EDGE ( 'NONE', *, *, #2283, .F. ) ;
#2451 = PRODUCT_DEFINITION_CONTEXT ( 'detailed design', #14741, 'design' ) ;
#2452 = AXIS2_PLACEMENT_3D ( 'NONE', #18673, #6523, #4562 ) ;
#2453 = ORIENTED_EDGE ( 'NONE', *, *, #10898, .F. ) ;
#2454 = ORIENTED_EDGE ( 'NONE', *, *, #14158, .T. ) ;
#2455 = CIRCLE ( 'NONE', #1971, 1.000000000000000888 ) ;
#2456 = FILL_AREA_STYLE ('',( #9991 ) ) ;
#2457 = AXIS2_PLACEMENT_3D ( 'NONE', #18199, #967, #7298 ) ;
#2458 = CARTESIAN_POINT ( 'NONE',  ( 53.48937290013659407, 129.7247684487574588, 283.6050404526570219 ) ) ;
#2459 = DIRECTION ( 'NONE',  ( 0.000000000000000000, 0.000000000000000000, -1.000000000000000000 ) ) ;
#2460 = AXIS2_PLACEMENT_3D ( 'NONE', #5180, #16506, #2247 ) ;
#2461 = EDGE_CURVE ( 'NONE', #17380, #19144, #4820, .T. ) ;
#2462 = PRESENTATION_STYLE_ASSIGNMENT (( #11950 ) ) ;
#2463 = CYLINDRICAL_SURFACE ( 'NONE', #14121, 10.00000000000000888 ) ;
#2464 = PLANE ( 'NONE',  #15705 ) ;
#2465 = CARTESIAN_POINT ( 'NONE',  ( 78.48937290013660117, 113.1299228374914208, 170.4174721992565082 ) ) ;
#2466 = CARTESIAN_POINT ( 'NONE',  ( 55.98937290013660828, 108.8727366810871899, 338.2196854716659118 ) ) ;
#2467 = CARTESIAN_POINT ( 'NONE',  ( 3.000000000000000000, 1.836909530733565148E-16, 12.50000000000000000 ) ) ;
#2468 = CARTESIAN_POINT ( 'NONE',  ( -36.00000000000000711, 6.000000000000000000, -22.00000000000000355 ) ) ;
#2469 = DIRECTION ( 'NONE',  ( 0.000000000000000000, 0.000000000000000000, -1.000000000000000000 ) ) ;
#2470 = ADVANCED_FACE ( 'NONE', ( #18037 ), #3935, .F. ) ;
#2471 = DIRECTION ( 'NONE',  ( 1.000000000000000000, 0.000000000000000000, 0.000000000000000000 ) ) ;
#2472 = DIRECTION ( 'NONE',  ( -0.000000000000000000, -0.000000000000000000, 1.000000000000000000 ) ) ;
#2473 =( LENGTH_UNIT ( ) NAMED_UNIT ( * ) SI_UNIT ( .MILLI., .METRE. ) );
#2474 = AXIS2_PLACEMENT_3D ( 'NONE', #16739, #8795, #19589 ) ;
#2475 = CIRCLE ( 'NONE', #12352, 9.000000000000007105 ) ;
#2476 = ADVANCED_FACE ( 'NONE', ( #11875 ), #8094, .T. ) ;
#2477 = STYLED_ITEM ( 'NONE', ( #9438 ), #14410 ) ;
#2478 = VERTEX_POINT ( 'NONE', #8786 ) ;
#2479 = ORIENTED_EDGE ( 'NONE', *, *, #11758, .T. ) ;
#2480 = VECTOR ( 'NONE', #14886, 1000.000000000000114 ) ;
#2481 = PLANE ( 'NONE',  #8412 ) ;
#2482 = VERTEX_POINT ( 'NONE', #916 ) ;
#2483 = VERTEX_POINT ( 'NONE', #2581 ) ;
#2484 =( GEOMETRIC_REPRESENTATION_CONTEXT ( 3 ) GLOBAL_UNCERTAINTY_ASSIGNED_CONTEXT ( ( #11217 ) ) GLOBAL_UNIT_ASSIGNED_CONTEXT ( ( #17449, #17358, #14261 ) ) REPRESENTATION_CONTEXT ( 'NONE', 'WORKASPACE' ) );
#2485 = DIRECTION ( 'NONE',  ( -0.000000000000000000, -0.000000000000000000, 1.000000000000000000 ) ) ;
#2486 = DIRECTION ( 'NONE',  ( -0.000000000000000000, -0.7791332379872890623, -0.6268583551835633649 ) ) ;
#2487 = APPLICATION_CONTEXT ( 'automotive_design' ) ;
#2488 = SURFACE_STYLE_USAGE ( .BOTH. , #13332 ) ;
#2489 = DIRECTION ( 'NONE',  ( 3.328238341717372086E-14, 0.000000000000000000, -1.000000000000000000 ) ) ;
#2490 = DIRECTION ( 'NONE',  ( 1.000000000000000000, 9.815121534730717399E-17, -0.000000000000000000 ) ) ;
#2491 = FACE_OUTER_BOUND ( 'NONE', #3037, .T. ) ;
#2492 = EDGE_CURVE ( 'NONE', #5205, #15503, #1006, .T. ) ;
#2493 = DIRECTION ( 'NONE',  ( 0.000000000000000000, 0.000000000000000000, -1.000000000000000000 ) ) ;
#2494 = DIRECTION ( 'NONE',  ( -1.000000000000000000, 0.000000000000000000, 0.000000000000000000 ) ) ;
#2495 = CYLINDRICAL_SURFACE ( 'NONE', #14834, 3.000000000000002665 ) ;
#2496 = FACE_OUTER_BOUND ( 'NONE', #10514, .T. ) ;
#2497 = ADVANCED_FACE ( 'NONE', ( #7449 ), #18749, .F. ) ;
#2498 = ORIENTED_EDGE ( 'NONE', *, *, #8382, .T. ) ;
#2499 = FILL_AREA_STYLE_COLOUR ( '', #293 ) ;
#2500 = CARTESIAN_POINT ( 'NONE',  ( 31.00000000000002842, 68.00000000000000000, 23.00000000000001066 ) ) ;
#2501 = EDGE_CURVE ( 'NONE', #19115, #1776, #3098, .T. ) ;
#2502 = ADVANCED_BREP_SHAPE_REPRESENTATION ( '', ( #1368, #1329, #1516, #2741 ), #5722 ) ;
#2503 = CARTESIAN_POINT ( 'NONE',  ( 153.4893729001366580, 80.91625508013694912, 250.0000000000000000 ) ) ;
#2504 = VERTEX_POINT ( 'NONE', #5890 ) ;
#2505 = AXIS2_PLACEMENT_3D ( 'NONE', #4417, #4316, #10595 ) ;
#2506 = ORIENTED_EDGE ( 'NONE', *, *, #4957, .T. ) ;
#2507 = CARTESIAN_POINT ( 'NONE',  ( -20.99999999999999645, 19.00000000000000000, 35.00000000000001421 ) ) ;
#2508 = CARTESIAN_POINT ( 'NONE',  ( 53.48937290013659407, 125.7247684487574588, 254.0000000000000000 ) ) ;
#2509 = UNCERTAINTY_MEASURE_WITH_UNIT (LENGTH_MEASURE( 1.000000000000000082E-05 ), #4318, 'distance_accuracy_value', 'NONE');
#2510 = VECTOR ( 'NONE', #6917, 1000.000000000000000 ) ;
#2511 = ORIENTED_EDGE ( 'NONE', *, *, #19315, .F. ) ;
#2512 = CARTESIAN_POINT ( 'NONE',  ( 498.8117674897343932, 191.8198460455371333, 24.99421986894476078 ) ) ;
#2513 = DIRECTION ( 'NONE',  ( -1.000000000000000000, -0.000000000000000000, -0.000000000000000000 ) ) ;
#2514 = FILL_AREA_STYLE ('',( #10349 ) ) ;
#2515 = DIRECTION ( 'NONE',  ( -1.000000000000000000, 0.000000000000000000, 0.000000000000000000 ) ) ;
#2516 = DIRECTION ( 'NONE',  ( -0.000000000000000000, -1.000000000000000000, -0.000000000000000000 ) ) ;
#2517 = CARTESIAN_POINT ( 'NONE',  ( -1.224646799147350495E-16, 41.00000000000000711, 6.000000000000000000 ) ) ;
#2518 =( NAMED_UNIT ( * ) SI_UNIT ( $, .STERADIAN. ) SOLID_ANGLE_UNIT ( ) );
#2519 = CARTESIAN_POINT ( 'NONE',  ( 153.4893729001366864, 123.1299228374914634, 79.58252780074349175 ) ) ;
#2520 = CARTESIAN_POINT ( 'NONE',  ( 53.48937290013658696, 122.8810204491430369, 322.0399576098686225 ) ) ;
#2521 = SHAPE_DEFINITION_REPRESENTATION ( #4647, #11716 ) ;
#2522 = EDGE_CURVE ( 'NONE', #8848, #7492, #3167, .T. ) ;
#2523 = FACE_OUTER_BOUND ( 'NONE', #16520, .T. ) ;
#2524 = EDGE_LOOP ( 'NONE', ( #16665, #9113, #6092, #1616 ) ) ;
#2525 = VECTOR ( 'NONE', #5531, 1000.000000000000000 ) ;
#2526 = ORIENTED_EDGE ( 'NONE', *, *, #12912, .T. ) ;
#2527 = VERTEX_POINT ( 'NONE', #14030 ) ;
#2528 = DIRECTION ( 'NONE',  ( 3.854941057726258312E-16, -0.000000000000000000, 1.000000000000000000 ) ) ;
#2529 = ORIENTED_EDGE ( 'NONE', *, *, #18180, .F. ) ;
#2530 = CARTESIAN_POINT ( 'NONE',  ( 0.000000000000000000, 216.7545334744432921, 0.000000000000000000 ) ) ;
#2531 = CARTESIAN_POINT ( 'NONE',  ( -40.00000000000000711, 0.000000000000000000, 26.00000000000000000 ) ) ;
#2532 = EDGE_LOOP ( 'NONE', ( #19110, #13908, #5128, #12475, #5947, #4332 ) ) ;
#2533 = CARTESIAN_POINT ( 'NONE',  ( 1.181929469892950335, 138.7545334744432637, 496.6642397995874489 ) ) ;
#2534 = ADVANCED_FACE ( 'NONE', ( #12169 ), #9737, .F. ) ;
#2535 = DIRECTION ( 'NONE',  ( 1.000000000000000000, 0.000000000000000000, -0.000000000000000000 ) ) ;
#2536 = CARTESIAN_POINT ( 'NONE',  ( -0.03824742239841866925, 139.0958210944198470, 488.5995842060523273 ) ) ;
#2537 = PRESENTATION_STYLE_ASSIGNMENT (( #18091 ) ) ;
#2538 = CARTESIAN_POINT ( 'NONE',  ( -22.99999999999999645, 68.00000000000000000, -31.00000000000005684 ) ) ;
#2539 = CARTESIAN_POINT ( 'NONE',  ( 53.48937290013658696, 126.1646452518344859, 280.0825295754780768 ) ) ;
#2540 = CARTESIAN_POINT ( 'NONE',  ( 3.000000000000000000, 41.00000000000000711, 9.013878188659973034 ) ) ;
#2541 = PLANE ( 'NONE',  #4033 ) ;
#2542 = FILL_AREA_STYLE_COLOUR ( '', #6913 ) ;
#2543 = CARTESIAN_POINT ( 'NONE',  ( 0.000000000000000000, 5.000000000000000888, 0.000000000000000000 ) ) ;
#2544 = EDGE_LOOP ( 'NONE', ( #8427, #9791 ) ) ;
#2545 = ADVANCED_FACE ( 'NONE', ( #4546 ), #8970, .T. ) ;
#2546 = PRESENTATION_LAYER_ASSIGNMENT (  '', '', ( #5517 ) ) ;
#2547 = ORIENTED_EDGE ( 'NONE', *, *, #2046, .T. ) ;
#2548 = ORIENTED_EDGE ( 'NONE', *, *, #7945, .F. ) ;
#2549 = ADVANCED_FACE ( 'NONE', ( #10826 ), #4646, .F. ) ;
#2550 = EDGE_LOOP ( 'NONE', ( #18379, #12059 ) ) ;
#2551 =( NAMED_UNIT ( * ) PLANE_ANGLE_UNIT ( ) SI_UNIT ( $, .RADIAN. ) );
#2552 = CARTESIAN_POINT ( 'NONE',  ( 31.00000000000000711, 68.00000000000000000, -30.99999999999999289 ) ) ;
#2553 = CARTESIAN_POINT ( 'NONE',  ( 178.4893729001365728, 103.1299228374914776, 29.36128450348865471 ) ) ;
#2554 = SURFACE_SIDE_STYLE ('',( #19648 ) ) ;
#2555 = PRESENTATION_STYLE_ASSIGNMENT (( #1281 ) ) ;
#2556 = SURFACE_STYLE_FILL_AREA ( #5872 ) ;
#2557 = AXIS2_PLACEMENT_3D ( 'NONE', #11929, #10385, #14610 ) ;
#2558 = CARTESIAN_POINT ( 'NONE',  ( 153.4893729001366864, 113.1299228374914634, 170.4174721992565082 ) ) ;
#2559 = CARTESIAN_POINT ( 'NONE',  ( -1.135258727068402823E-15, 152.4824555358011082, 478.3411705753777596 ) ) ;
#2560 = EDGE_CURVE ( 'NONE', #11965, #11435, #15589, .T. ) ;
#2561 = CYLINDRICAL_SURFACE ( 'NONE', #5055, 3.299999999999997158 ) ;
#2562 = CARTESIAN_POINT ( 'NONE',  ( -1.000000000000004885, 146.8256012863087108, 507.0490161104376057 ) ) ;
#2563 = DIRECTION ( 'NONE',  ( 0.000000000000000000, 0.000000000000000000, 1.000000000000000000 ) ) ;
#2564 = SURFACE_SIDE_STYLE ('',( #7618 ) ) ;
#2565 = CARTESIAN_POINT ( 'NONE',  ( 55.48937290013660117, 127.7247684487574588, 370.0000000000000000 ) ) ;
#2566 = ADVANCED_FACE ( 'NONE', ( #12901 ), #14116, .F. ) ;
#2567 = VERTEX_POINT ( 'NONE', #207 ) ;
#2568 = ORIENTED_EDGE ( 'NONE', *, *, #18752, .F. ) ;
#2569 = ORIENTED_EDGE ( 'NONE', *, *, #18097, .T. ) ;
#2570 = AXIS2_PLACEMENT_3D ( 'NONE', #19503, #5221, #2102 ) ;
#2571 = EDGE_CURVE ( 'NONE', #20182, #10544, #7838, .T. ) ;
#2572 = CARTESIAN_POINT ( 'NONE',  ( 0.000000000000000000, 368.2663108437010919, -142.2176018917206761 ) ) ;
#2573 = VERTEX_POINT ( 'NONE', #1621 ) ;
#2574 = EDGE_LOOP ( 'NONE', ( #1496, #6237, #15794, #7280 ) ) ;
#2575 = DIRECTION ( 'NONE',  ( 0.000000000000000000, 0.000000000000000000, 1.000000000000000000 ) ) ;
#2576 = ADVANCED_FACE ( 'NONE', ( #11335 ), #12578, .T. ) ;
#2577 = SURFACE_SIDE_STYLE ('',( #18241 ) ) ;
#2578 = LINE ( 'NONE', #13811, #9570 ) ;
#2579 = SURFACE_STYLE_USAGE ( .BOTH. , #11774 ) ;
#2580 = EDGE_CURVE ( 'NONE', #5279, #13880, #16108, .T. ) ;
#2581 = CARTESIAN_POINT ( 'NONE',  ( 98.48937290013662960, 103.1299228374914208, 79.58252780074349175 ) ) ;
#2582 = DIRECTION ( 'NONE',  ( 0.000000000000000000, 1.000000000000000000, 0.000000000000000000 ) ) ;
#2583 = CARTESIAN_POINT ( 'NONE',  ( -31.00000000000007105, 0.000000000000000000, 23.00000000000000000 ) ) ;
#2584 = ADVANCED_FACE ( 'NONE', ( #6302 ), #4859, .T. ) ;
#2585 = CARTESIAN_POINT ( 'NONE',  ( 34.99999999999997868, 0.000000000000000000, -40.00000000000000711 ) ) ;
#2586 = CARTESIAN_POINT ( 'NONE',  ( 0.000000000000000000, 138.7545334744432637, 496.6642397995874489 ) ) ;
#2587 = CARTESIAN_POINT ( 'NONE',  ( -80.45457315056674474, 138.8734935819628049, 489.4082602761224621 ) ) ;
#2588 = VECTOR ( 'NONE', #20327, 1000.000000000000000 ) ;
#2589 = ORIENTED_EDGE ( 'NONE', *, *, #14911, .F. ) ;
#2590 = STYLED_ITEM ( 'NONE', ( #19408 ), #11064 ) ;
#2591 = DIRECTION ( 'NONE',  ( 0.000000000000000000, 0.000000000000000000, -1.000000000000000000 ) ) ;
#2592 = DIRECTION ( 'NONE',  ( -0.000000000000000000, 0.000000000000000000, 1.000000000000000000 ) ) ;
#2593 = CARTESIAN_POINT ( 'NONE',  ( -26.00000000000000000, 11.00000000000000000, 40.00000000000000711 ) ) ;
#2594 = ORIENTED_EDGE ( 'NONE', *, *, #8255, .T. ) ;
#2595 = ORIENTED_EDGE ( 'NONE', *, *, #19556, .T. ) ;
#2596 = VECTOR ( 'NONE', #16608, 1000.000000000000000 ) ;
#2597 = AXIS2_PLACEMENT_3D ( 'NONE', #1017, #16646, #19785 ) ;
#2599 = VERTEX_POINT ( 'NONE', #13009 ) ;
#2598 = AXIS2_PLACEMENT_3D ( 'NONE', #18469, #9002, #4363 ) ;
#2600 = ADVANCED_FACE ( 'NONE', ( #11042 ), #12720, .T. ) ;
#2601 = FACE_OUTER_BOUND ( 'NONE', #10394, .T. ) ;
#2602 = DIRECTION ( 'NONE',  ( 0.000000000000000000, 1.000000000000000000, 0.000000000000000000 ) ) ;
#2603 = EDGE_LOOP ( 'NONE', ( #6537, #8500, #14463, #17208, #1300, #7777, #11421, #14190 ) ) ;
#2604 = FACE_OUTER_BOUND ( 'NONE', #18593, .T. ) ;
#2605 = CARTESIAN_POINT ( 'NONE',  ( -80.68769470327367799, 139.4951205324793477, 500.2397034702902374 ) ) ;
#2606 = DIRECTION ( 'NONE',  ( -1.000000000000000000, 0.000000000000000000, 7.715811803773179210E-14 ) ) ;
#2607 = SURFACE_SIDE_STYLE ('',( #8899 ) ) ;
#2608 = EDGE_CURVE ( 'NONE', #7143, #6864, #14428, .T. ) ;
#2609 = EDGE_CURVE ( 'NONE', #9862, #14625, #3300, .T. ) ;
#2610 = LINE ( 'NONE', #10449, #4751 ) ;
#2611 = FACE_OUTER_BOUND ( 'NONE', #12353, .T. ) ;
#2612 = ORIENTED_EDGE ( 'NONE', *, *, #12814, .T. ) ;
#2613 = FACE_OUTER_BOUND ( 'NONE', #17692, .T. ) ;
#2614 = DIRECTION ( 'NONE',  ( 1.000000000000000000, 0.000000000000000000, -1.017652531801993019E-13 ) ) ;
#2615 =( NAMED_UNIT ( * ) PLANE_ANGLE_UNIT ( ) SI_UNIT ( $, .RADIAN. ) );
#2616 = AXIS2_PLACEMENT_3D ( 'NONE', #9448, #15756, #18805 ) ;
#2617 = APPLICATION_PROTOCOL_DEFINITION ( 'draft international standard', 'automotive_design', 1998, #11975 ) ;
#2618 = VECTOR ( 'NONE', #5705, 1000.000000000000000 ) ;
#2619 = ORIENTED_EDGE ( 'NONE', *, *, #17461, .T. ) ;
#2620 = VERTEX_POINT ( 'NONE', #6716 ) ;
#2621 = EDGE_LOOP ( 'NONE', ( #20309, #6145, #6277, #1410 ) ) ;
#2622 = ORIENTED_EDGE ( 'NONE', *, *, #12264, .T. ) ;
#2623 = DIRECTION ( 'NONE',  ( -0.000000000000000000, -1.000000000000000000, -0.000000000000000000 ) ) ;
#2624 = ORIENTED_EDGE ( 'NONE', *, *, #9358, .T. ) ;
#2625 = DIRECTION ( 'NONE',  ( 1.000000000000000000, 5.889072920838430686E-16, -0.000000000000000000 ) ) ;
#2626 = PRESENTATION_LAYER_ASSIGNMENT (  '', '', ( #17105 ) ) ;
#2627 = VERTEX_POINT ( 'NONE', #1934 ) ;
#2628 = CIRCLE ( 'NONE', #13506, 18.50000000000000000 ) ;
#2629 = DIRECTION ( 'NONE',  ( -1.000000000000000000, -2.135044278125301096E-16, -0.000000000000000000 ) ) ;
#2630 = EDGE_CURVE ( 'NONE', #13356, #14748, #17638, .T. ) ;
#2631 = VECTOR ( 'NONE', #15805, 1000.000000000000000 ) ;
#2632 = PRESENTATION_STYLE_ASSIGNMENT (( #4291 ) ) ;
#2633 = LINE ( 'NONE', #4203, #5593 ) ;
#2634 = CARTESIAN_POINT ( 'NONE',  ( 1.224999999999999867, 0.000000000000000000, 0.000000000000000000 ) ) ;
#2635 = FILL_AREA_STYLE_COLOUR ( '', #10508 ) ;
#2636 = SURFACE_STYLE_FILL_AREA ( #13481 ) ;
#2637 = DIRECTION ( 'NONE',  ( -7.715811803773179210E-14, 0.000000000000000000, -1.000000000000000000 ) ) ;
#2638 = DIRECTION ( 'NONE',  ( 0.000000000000000000, -1.000000000000000000, 0.000000000000000000 ) ) ;
#2639 = CARTESIAN_POINT ( 'NONE',  ( 0.000000000000000000, 5.000000000000000888, -150.0000000000000000 ) ) ;
#2640 = SHAPE_REPRESENTATION_RELATIONSHIP ( 'NONE' , 'NONE' ,  #18121, #13084 ) ;
#2641 =( NAMED_UNIT ( * ) PLANE_ANGLE_UNIT ( ) SI_UNIT ( $, .RADIAN. ) );
#2642 = LINE ( 'NONE', #18309, #12582 ) ;
#2643 = DIRECTION ( 'NONE',  ( 0.000000000000000000, 7.137148015447440312E-15, -1.000000000000000000 ) ) ;
#2644 = PRESENTATION_STYLE_ASSIGNMENT (( #12225 ) ) ;
#2645 = DIRECTION ( 'NONE',  ( -0.000000000000000000, 1.000000000000000000, -0.000000000000000000 ) ) ;
#2646 = ORIENTED_EDGE ( 'NONE', *, *, #18943, .T. ) ;
#2647 = AXIS2_PLACEMENT_3D ( 'NONE', #10573, #4386, #15424 ) ;
#2648 = VECTOR ( 'NONE', #3850, 1000.000000000000000 ) ;
#2649 = ORIENTED_EDGE ( 'NONE', *, *, #9103, .T. ) ;
#2650 = UNCERTAINTY_MEASURE_WITH_UNIT (LENGTH_MEASURE( 1.000000000000000082E-05 ), #6675, 'distance_accuracy_value', 'NONE');
#2651 = ORIENTED_EDGE ( 'NONE', *, *, #13715, .F. ) ;
#2652 = VECTOR ( 'NONE', #1851, 1000.000000000000000 ) ;
#2653 = ORIENTED_EDGE ( 'NONE', *, *, #9894, .T. ) ;
#2654 =( LENGTH_UNIT ( ) NAMED_UNIT ( * ) SI_UNIT ( .MILLI., .METRE. ) );
#2655 = CARTESIAN_POINT ( 'NONE',  ( -0.000000000000000000, 167.9162550801369491, 250.0000000000000000 ) ) ;
#2656 = DIRECTION ( 'NONE',  ( 1.000000000000000000, 0.000000000000000000, 0.000000000000000000 ) ) ;
#2657 = PLANE ( 'NONE',  #14615 ) ;
#2658 = CARTESIAN_POINT ( 'NONE',  ( -34.99999999999996447, 0.000000000000000000, 40.00000000000000711 ) ) ;
#2659 = VECTOR ( 'NONE', #16239, 1000.000000000000000 ) ;
#2660 = CARTESIAN_POINT ( 'NONE',  ( 35.00000000000003553, -20.00000000000000000, -20.99999999999999645 ) ) ;
#2661 = MECHANICAL_DESIGN_GEOMETRIC_PRESENTATION_REPRESENTATION (  '', ( #27 ), #13859 ) ;
#2662 = DIRECTION ( 'NONE',  ( -1.000000000000000000, 0.000000000000000000, 7.715811803773179210E-14 ) ) ;
#2663 = LINE ( 'NONE', #7428, #3839 ) ;
#2664 = LINE ( 'NONE', #18423, #9988 ) ;
#2665 = FILL_AREA_STYLE_COLOUR ( '', #13813 ) ;
#2666 = DIRECTION ( 'NONE',  ( 0.000000000000000000, -1.000000000000000000, 0.000000000000000000 ) ) ;
#2667 = PRODUCT_RELATED_PRODUCT_CATEGORY ( 'part', '', ( #5172 ) ) ;
#2668 = CARTESIAN_POINT ( 'NONE',  ( 109.4893729001366012, 127.7247684487574588, 370.0000000000000000 ) ) ;
#2669 = CARTESIAN_POINT ( 'NONE',  ( -26.00000000000000000, 11.00000000000000000, 40.00000000000000711 ) ) ;
#2670 = ADVANCED_FACE ( 'NONE', ( #17322 ), #14525, .F. ) ;
#2671 = STYLED_ITEM ( 'NONE', ( #6086 ), #17188 ) ;
#2672 = ORIENTED_EDGE ( 'NONE', *, *, #17630, .T. ) ;
#2673 = DIRECTION ( 'NONE',  ( 0.000000000000000000, 0.000000000000000000, -1.000000000000000000 ) ) ;
#2674 = AXIS2_PLACEMENT_3D ( 'NONE', #8610, #20214, #15499 ) ;
#2675 = ORIENTED_EDGE ( 'NONE', *, *, #17306, .T. ) ;
#2676 = ORIENTED_EDGE ( 'NONE', *, *, #1826, .F. ) ;
#2677 = LINE ( 'NONE', #2878, #10726 ) ;
#2678 = LINE ( 'NONE', #15478, #5405 ) ;
#2679 = UNCERTAINTY_MEASURE_WITH_UNIT (LENGTH_MEASURE( 1.000000000000000082E-05 ), #20149, 'distance_accuracy_value', 'NONE');
#2680 = CARTESIAN_POINT ( 'NONE',  ( 0.000000000000000000, 219.7545334744432921, 512.1946179577817020 ) ) ;
#2681 =( NAMED_UNIT ( * ) PLANE_ANGLE_UNIT ( ) SI_UNIT ( $, .RADIAN. ) );
#2682 = FILL_AREA_STYLE_COLOUR ( '', #8047 ) ;
#2683 = ADVANCED_FACE ( 'NONE', ( #15786 ), #6503, .T. ) ;
#2684 = DIRECTION ( 'NONE',  ( 0.000000000000000000, 1.000000000000000000, 0.000000000000000000 ) ) ;
#2685 = AXIS2_PLACEMENT_3D ( 'NONE', #9853, #6789, #14705 ) ;
#2686 = DIRECTION ( 'NONE',  ( 0.000000000000000000, 0.000000000000000000, -1.000000000000000000 ) ) ;
#2687 = DIRECTION ( 'NONE',  ( 1.000000000000000000, 0.000000000000000000, 0.000000000000000000 ) ) ;
#2688 = CARTESIAN_POINT ( 'NONE',  ( -80.38411152862499875, 139.8075349053433740, 489.3561120975041376 ) ) ;
#2689 = DIRECTION ( 'NONE',  ( 1.000000000000000000, 0.000000000000000000, -0.000000000000000000 ) ) ;
#2690 = EDGE_CURVE ( 'NONE', #4515, #8097, #13699, .T. ) ;
#2691 = AXIS2_PLACEMENT_3D ( 'NONE', #4919, #1382, #12764 ) ;
#2692 = ORIENTED_EDGE ( 'NONE', *, *, #12681, .T. ) ;
#2693 = CARTESIAN_POINT ( 'NONE',  ( -1.000000000000001554, 152.4824555358010798, 509.3921618609452935 ) ) ;
#2694 = EDGE_CURVE ( 'NONE', #6321, #14904, #15352, .T. ) ;
#2695 = EDGE_CURVE ( 'NONE', #3271, #8713, #99, .T. ) ;
#2696 = VERTEX_POINT ( 'NONE', #4953 ) ;
#2697 = CIRCLE ( 'NONE', #16243, 3.000000000000002665 ) ;
#2698 = PRESENTATION_LAYER_ASSIGNMENT (  '', '', ( #9279 ) ) ;
#2699 = UNCERTAINTY_MEASURE_WITH_UNIT (LENGTH_MEASURE( 1.000000000000000082E-05 ), #8225, 'distance_accuracy_value', 'NONE');
#2700 = COLOUR_RGB ( '', 0.40784314, 0.44705882, 0.49803922) ;
#2701 = SURFACE_SIDE_STYLE ('',( #10542 ) ) ;
#2702 = UNCERTAINTY_MEASURE_WITH_UNIT (LENGTH_MEASURE( 1.000000000000000082E-05 ), #7069, 'distance_accuracy_value', 'NONE');
#2703 = ORIENTED_EDGE ( 'NONE', *, *, #7218, .F. ) ;
#2704 = CARTESIAN_POINT ( 'NONE',  ( 1.530757942277970587E-15, 0.000000000000000000, 24.99999999999999645 ) ) ;
#2705 = SURFACE_STYLE_USAGE ( .BOTH. , #16843 ) ;
#2707 = EDGE_CURVE ( 'NONE', #4851, #13965, #11227, .T. ) ;
#2706 = FILL_AREA_STYLE ('',( #2400 ) ) ;
#2708 = STYLED_ITEM ( 'NONE', ( #18301 ), #3313 ) ;
#2709 = COLOUR_RGB ( '', 0.66274510, 0.83137255, 0.94901961) ;
#2710 = DIRECTION ( 'NONE',  ( -0.000000000000000000, -0.000000000000000000, -1.000000000000000000 ) ) ;
#2711 =( NAMED_UNIT ( * ) PLANE_ANGLE_UNIT ( ) SI_UNIT ( $, .RADIAN. ) );
#2712 = LINE ( 'NONE', #12415, #8057 ) ;
#2713 = ORIENTED_EDGE ( 'NONE', *, *, #18956, .T. ) ;
#2714 = SURFACE_STYLE_FILL_AREA ( #13748 ) ;
#2715 =( GEOMETRIC_REPRESENTATION_CONTEXT ( 3 ) GLOBAL_UNCERTAINTY_ASSIGNED_CONTEXT ( ( #621 ) ) GLOBAL_UNIT_ASSIGNED_CONTEXT ( ( #1117, #18446, #13726 ) ) REPRESENTATION_CONTEXT ( 'NONE', 'WORKASPACE' ) );
#2716 = VECTOR ( 'NONE', #14585, 1000.000000000000114 ) ;
#2717 = SURFACE_STYLE_FILL_AREA ( #16762 ) ;
#2718 =( LENGTH_UNIT ( ) NAMED_UNIT ( * ) SI_UNIT ( .MILLI., .METRE. ) );
#2719 = ORIENTED_EDGE ( 'NONE', *, *, #7049, .T. ) ;
#2720 = ORIENTED_EDGE ( 'NONE', *, *, #17607, .T. ) ;
#2721 = VECTOR ( 'NONE', #16255, 1000.000000000000000 ) ;
#2722 = EDGE_CURVE ( 'NONE', #13882, #19875, #16032, .T. ) ;
#2723 = VERTEX_POINT ( 'NONE', #6923 ) ;
#2724 = ORIENTED_EDGE ( 'NONE', *, *, #196, .T. ) ;
#2725 = VECTOR ( 'NONE', #2886, 1000.000000000000000 ) ;
#2726 = ORIENTED_EDGE ( 'NONE', *, *, #18467, .F. ) ;
#2727 = LINE ( 'NONE', #7488, #13051 ) ;
#2728 = EDGE_LOOP ( 'NONE', ( #17079, #11265, #11947, #5482 ) ) ;
#2729 = CARTESIAN_POINT ( 'NONE',  ( -31.00000000000001776, 10.00000000000000000, 31.00000000000000000 ) ) ;
#2730 = VECTOR ( 'NONE', #1359, 1000.000000000000000 ) ;
#2731 = FACE_OUTER_BOUND ( 'NONE', #3460, .T. ) ;
#2732 = VECTOR ( 'NONE', #8929, 1000.000000000000000 ) ;
#2733 = DIRECTION ( 'NONE',  ( 0.000000000000000000, -1.000000000000000000, 0.000000000000000000 ) ) ;
#2734 = LINE ( 'NONE', #18490, #3378 ) ;
#2735 = CARTESIAN_POINT ( 'NONE',  ( 5.945602903476760126, -13.89560290347679938, -1.701720561796553076E-15 ) ) ;
#2736 = DIRECTION ( 'NONE',  ( -0.000000000000000000, -1.000000000000000000, -0.000000000000000000 ) ) ;
#2737 = CARTESIAN_POINT ( 'NONE',  ( 37.00000000000003553, 3.000000000000000000, 20.00000000000000000 ) ) ;
#2738 = LINE ( 'NONE', #8739, #3421 ) ;
#2739 = CIRCLE ( 'NONE', #18194, 2.500000000000002220 ) ;
#2740 = EDGE_CURVE ( 'NONE', #18268, #1517, #13501, .T. ) ;
#2741 = AXIS2_PLACEMENT_3D ( 'NONE', #5042, #3500, #8234 ) ;
#2742 = CARTESIAN_POINT ( 'NONE',  ( 10.00000000000000000, 301.0487089519832011, -80.00000000000387956 ) ) ;
#2743 = PLANE ( 'NONE',  #5032 ) ;
#2744 = LINE ( 'NONE', #10387, #17524 ) ;
#2745 = DIRECTION ( 'NONE',  ( 0.000000000000000000, 0.000000000000000000, 1.000000000000000000 ) ) ;
#2746 =( NAMED_UNIT ( * ) SI_UNIT ( $, .STERADIAN. ) SOLID_ANGLE_UNIT ( ) );
#2747 = CARTESIAN_POINT ( 'NONE',  ( -31.00000000000003553, 19.00000000000000000, -21.00000000000000000 ) ) ;
#2748 = LINE ( 'NONE', #2543, #16157 ) ;
#2749 = MECHANICAL_DESIGN_GEOMETRIC_PRESENTATION_REPRESENTATION (  '', ( #4399 ), #7381 ) ;
#2750 = ORIENTED_EDGE ( 'NONE', *, *, #5322, .T. ) ;
#2751 = AXIS2_PLACEMENT_3D ( 'NONE', #18914, #10991, #262 ) ;
#2752 = ORIENTED_EDGE ( 'NONE', *, *, #1627, .T. ) ;
#2753 = ORIENTED_EDGE ( 'NONE', *, *, #16919, .T. ) ;
#2754 = PRESENTATION_LAYER_ASSIGNMENT (  '', '', ( #3425 ) ) ;
#2755 = EDGE_LOOP ( 'NONE', ( #5305, #2479, #4849, #16937 ) ) ;
#2756 = FILL_AREA_STYLE ('',( #1383 ) ) ;
#2757 = MECHANICAL_DESIGN_GEOMETRIC_PRESENTATION_REPRESENTATION (  '', ( #15962 ), #1428 ) ;
#2758 = ORIENTED_EDGE ( 'NONE', *, *, #3216, .F. ) ;
#2759 = CARTESIAN_POINT ( 'NONE',  ( 22.99999999999995737, 0.000000000000000000, -33.99999999999998579 ) ) ;
#2760 = CARTESIAN_POINT ( 'NONE',  ( -75.00000000000000000, 368.2663108437010919, -142.2176018917206761 ) ) ;
#2761 = ORIENTED_EDGE ( 'NONE', *, *, #9735, .F. ) ;
#2762 = AXIS2_PLACEMENT_3D ( 'NONE', #9949, #14581, #6782 ) ;
#2763 = DIRECTION ( 'NONE',  ( 1.000000000000000000, 0.000000000000000000, 3.854941057726246479E-16 ) ) ;
#2764 = DIRECTION ( 'NONE',  ( 1.000000000000000000, 0.000000000000000000, -0.000000000000000000 ) ) ;
#2765 = FILL_AREA_STYLE ('',( #4528 ) ) ;
#2766 = PRESENTATION_STYLE_ASSIGNMENT (( #17090 ) ) ;
#2767 = FILL_AREA_STYLE_COLOUR ( '', #15846 ) ;
#2768 = COLOUR_RGB ( '', 0.31764706, 0.68627451, 0.89019608) ;
#2769 = CIRCLE ( 'NONE', #18548, 8.000000000000007105 ) ;
#2770 = CARTESIAN_POINT ( 'NONE',  ( -37.00000000000000000, 68.00000000000000000, -22.99999999999999645 ) ) ;
#2771 = CIRCLE ( 'NONE', #2452, 15.14120580695350071 ) ;
#2772 = ADVANCED_FACE ( 'NONE', ( #5264 ), #2352, .F. ) ;
#2773 = STYLED_ITEM ( 'NONE', ( #11963 ), #19583 ) ;
#2774 = VERTEX_POINT ( 'NONE', #17817 ) ;
#2775 = PRESENTATION_LAYER_ASSIGNMENT (  '', '', ( #13642 ) ) ;
#2776 = ORIENTED_EDGE ( 'NONE', *, *, #1175, .F. ) ;
#2777 = MECHANICAL_DESIGN_GEOMETRIC_PRESENTATION_REPRESENTATION (  '', ( #6756 ), #14306 ) ;
#2778 = ORIENTED_EDGE ( 'NONE', *, *, #1445, .T. ) ;
#2779 = VERTEX_POINT ( 'NONE', #3715 ) ;
#2780 = LINE ( 'NONE', #15476, #6810 ) ;
#2781 =( GEOMETRIC_REPRESENTATION_CONTEXT ( 3 ) GLOBAL_UNCERTAINTY_ASSIGNED_CONTEXT ( ( #17743 ) ) GLOBAL_UNIT_ASSIGNED_CONTEXT ( ( #2162, #3629, #5077 ) ) REPRESENTATION_CONTEXT ( 'NONE', 'WORKASPACE' ) );
#2782 = CARTESIAN_POINT ( 'NONE',  ( 53.48937290013659407, 208.2227610943810134, 346.7612763259490407 ) ) ;
#2783 = CYLINDRICAL_SURFACE ( 'NONE', #12557, 1.000000000000015987 ) ;
#2784 =( GEOMETRIC_REPRESENTATION_CONTEXT ( 3 ) GLOBAL_UNCERTAINTY_ASSIGNED_CONTEXT ( ( #854 ) ) GLOBAL_UNIT_ASSIGNED_CONTEXT ( ( #13674, #16868, #4289 ) ) REPRESENTATION_CONTEXT ( 'NONE', 'WORKASPACE' ) );
#2785 = FACE_OUTER_BOUND ( 'NONE', #13609, .T. ) ;
#2786 = COLOUR_RGB ( '', 0.40784314, 0.44705882, 0.49803922) ;
#2787 = DIRECTION ( 'NONE',  ( 1.000000000000000000, -0.000000000000000000, -0.000000000000000000 ) ) ;
#2788 =( LENGTH_UNIT ( ) NAMED_UNIT ( * ) SI_UNIT ( .MILLI., .METRE. ) );
#2789 = DIRECTION ( 'NONE',  ( -0.000000000000000000, -1.000000000000000000, -0.000000000000000000 ) ) ;
#2790 = CARTESIAN_POINT ( 'NONE',  ( 178.4893729001365443, 167.9162550801369491, 0.000000000000000000 ) ) ;
#2791 = ADVANCED_FACE ( 'NONE', ( #13115 ), #8117, .T. ) ;
#2792 = AXIS2_PLACEMENT_3D ( 'NONE', #8337, #8139, #6590 ) ;
#2793 = DIRECTION ( 'NONE',  ( 0.000000000000000000, 0.000000000000000000, 1.000000000000000000 ) ) ;
#2794 = LINE ( 'NONE', #4346, #14233 ) ;
#2795 = CARTESIAN_POINT ( 'NONE',  ( 463.8334540492693350, 191.8198460455371333, 168.2339398819845826 ) ) ;
#2796 = ORIENTED_EDGE ( 'NONE', *, *, #16071, .F. ) ;
#2797 = CARTESIAN_POINT ( 'NONE',  ( 0.000000000000000000, 0.000000000000000000, -150.0000000000000000 ) ) ;
#2798 = CYLINDRICAL_SURFACE ( 'NONE', #7716, 3.999999999999996447 ) ;
#2799 = CIRCLE ( 'NONE', #20262, 13.95000000000000107 ) ;
#2800 = AXIS2_PLACEMENT_3D ( 'NONE', #16675, #2528, #4380 ) ;
#2801 = EDGE_CURVE ( 'NONE', #5440, #6498, #2031, .T. ) ;
#2802 = ORIENTED_EDGE ( 'NONE', *, *, #18707, .F. ) ;
#2803 = EDGE_CURVE ( 'NONE', #3148, #11681, #9997, .T. ) ;
#2804 = ORIENTED_EDGE ( 'NONE', *, *, #4709, .T. ) ;
#2805 =( NAMED_UNIT ( * ) SI_UNIT ( $, .STERADIAN. ) SOLID_ANGLE_UNIT ( ) );
#2806 = DIRECTION ( 'NONE',  ( 0.000000000000000000, 0.000000000000000000, 1.000000000000000000 ) ) ;
#2807 = ORIENTED_EDGE ( 'NONE', *, *, #5374, .F. ) ;
#2808 = CARTESIAN_POINT ( 'NONE',  ( 53.48937290013659407, 125.7247684487574588, 252.0000000000000000 ) ) ;
#2809 = AXIS2_PLACEMENT_3D ( 'NONE', #8873, #5388, #5576 ) ;
#2810 = CARTESIAN_POINT ( 'NONE',  ( 423.8334540492694487, 191.8198460455371333, 168.2339398819845826 ) ) ;
#2811 = VECTOR ( 'NONE', #13808, 1000.000000000000000 ) ;
#2812 = EDGE_CURVE ( 'NONE', #18079, #12831, #9056, .T. ) ;
#2813 = FACE_OUTER_BOUND ( 'NONE', #16072, .T. ) ;
#2814 = PRESENTATION_STYLE_ASSIGNMENT (( #15191 ) ) ;
#2815 = VERTEX_POINT ( 'NONE', #896 ) ;
#2816 = CYLINDRICAL_SURFACE ( 'NONE', #3243, 0.9999999999999965583 ) ;
#2817 = EDGE_CURVE ( 'NONE', #10868, #18646, #13413, .T. ) ;
#2818 = CARTESIAN_POINT ( 'NONE',  ( 0.000000000000000000, 16.00000000000000000, 0.000000000000000000 ) ) ;
#2819 = PLANE ( 'NONE',  #8367 ) ;
#2820 = PRODUCT_CONTEXT ( 'NONE', #3930, 'mechanical' ) ;
#2821 = PRODUCT_DEFINITION_SHAPE ( 'NONE', 'NONE',  #20382 ) ;
#2822 = EDGE_LOOP ( 'NONE', ( #4254, #17363, #6472, #2021, #9117, #3380, #13904, #16146, #10816, #12588, #7786, #2952, #2232, #18985, #15182, #797 ) ) ;
#2823 = ORIENTED_EDGE ( 'NONE', *, *, #20202, .F. ) ;
#2824 = DIRECTION ( 'NONE',  ( 1.000000000000000000, 0.000000000000000000, -0.000000000000000000 ) ) ;
#2825 = EDGE_LOOP ( 'NONE', ( #8917, #15650, #1743, #15687 ) ) ;
#2826 = ORIENTED_EDGE ( 'NONE', *, *, #5936, .F. ) ;
#2827 = EDGE_CURVE ( 'NONE', #9164, #2774, #9756, .T. ) ;
#2828 = ORIENTED_EDGE ( 'NONE', *, *, #5623, .F. ) ;
#2829 = CARTESIAN_POINT ( 'NONE',  ( 5.687501635565830327, 0.000000000000000000, 0.000000000000000000 ) ) ;
#2830 = ORIENTED_EDGE ( 'NONE', *, *, #20322, .T. ) ;
#2831 = LINE ( 'NONE', #4198, #13963 ) ;
#2832 = EDGE_LOOP ( 'NONE', ( #171, #19097 ) ) ;
#2833 = EDGE_CURVE ( 'NONE', #10340, #1663, #13714, .T. ) ;
#2834 = CARTESIAN_POINT ( 'NONE',  ( 468.8334540492694487, 214.2156642432025251, 245.0000000000000000 ) ) ;
#2835 = SURFACE_STYLE_FILL_AREA ( #16774 ) ;
#2836 =( NAMED_UNIT ( * ) PLANE_ANGLE_UNIT ( ) SI_UNIT ( $, .RADIAN. ) );
#2837 = CYLINDRICAL_SURFACE ( 'NONE', #12259, 10.00000000000000888 ) ;
#2838 = EDGE_CURVE ( 'NONE', #15103, #2973, #14831, .T. ) ;
#2839 = CARTESIAN_POINT ( 'NONE',  ( -77.99033078109007988, 127.7247684487574304, 357.7985149490353933 ) ) ;
#2840 = DIRECTION ( 'NONE',  ( 0.000000000000000000, 0.000000000000000000, -1.000000000000000000 ) ) ;
#2841 = LINE ( 'NONE', #4206, #11127 ) ;
#2842 = CARTESIAN_POINT ( 'NONE',  ( 498.8334540492693918, 191.8198460455371333, 168.2339398819845826 ) ) ;
#2843 = CARTESIAN_POINT ( 'NONE',  ( -26.00000000000002842, 3.000000000000000000, 31.00000000000003908 ) ) ;
#2844 = CIRCLE ( 'NONE', #18647, 10.00000000000000888 ) ;
#2845 = DIRECTION ( 'NONE',  ( 0.000000000000000000, -1.000000000000000000, 0.000000000000000000 ) ) ;
#2846 = CARTESIAN_POINT ( 'NONE',  ( 423.8334540492694487, 191.8198460455371333, 91.76606011801541740 ) ) ;
#2847 = DIRECTION ( 'NONE',  ( 1.000000000000000000, 0.000000000000000000, 0.000000000000000000 ) ) ;
#2848 = DIRECTION ( 'NONE',  ( -0.000000000000000000, -1.000000000000000000, 0.000000000000000000 ) ) ;
#2849 = DIRECTION ( 'NONE',  ( 1.000000000000000000, 0.000000000000000000, 0.000000000000000000 ) ) ;
#2850 = EDGE_LOOP ( 'NONE', ( #16383, #16030, #12262, #12254 ) ) ;
#2852 = ORIENTED_EDGE ( 'NONE', *, *, #1268, .T. ) ;
#2851 = ADVANCED_FACE ( 'NONE', ( #17924 ), #2464, .T. ) ;
#2853 = PLANE ( 'NONE',  #16692 ) ;
#2854 = EDGE_LOOP ( 'NONE', ( #16353, #18066, #6274, #4703 ) ) ;
#2855 = CARTESIAN_POINT ( 'NONE',  ( -38.50085094405407204, 193.0431417881923153, 505.3921618609452935 ) ) ;
#2856 = SURFACE_STYLE_USAGE ( .BOTH. , #11178 ) ;
#2857 = EDGE_LOOP ( 'NONE', ( #1695, #3174 ) ) ;
#2858 = EDGE_CURVE ( 'NONE', #3611, #10328, #7312, .T. ) ;
#2859 = FACE_BOUND ( 'NONE', #15325, .T. ) ;
#2860 = FILL_AREA_STYLE ('',( #10707 ) ) ;
#2861 = DIRECTION ( 'NONE',  ( 0.000000000000000000, 0.000000000000000000, -1.000000000000000000 ) ) ;
#2862 = CARTESIAN_POINT ( 'NONE',  ( -1.845421771225094876, 62.39699037330763076, 9.323305159997635982 ) ) ;
#2863 = CYLINDRICAL_SURFACE ( 'NONE', #16746, 3.300000000000025135 ) ;
#2864 = EDGE_CURVE ( 'NONE', #3254, #4150, #10418, .T. ) ;
#2865 = CARTESIAN_POINT ( 'NONE',  ( 18.99999999999998224, 8.000000000000000000, -35.99999999999999289 ) ) ;
#2866 = PLANE ( 'NONE',  #18760 ) ;
#2867 = DIRECTION ( 'NONE',  ( 1.000000000000000000, 0.000000000000000000, 0.000000000000000000 ) ) ;
#2868 = MECHANICAL_DESIGN_GEOMETRIC_PRESENTATION_REPRESENTATION (  '', ( #10452 ), #14394 ) ;
#2869 = DIRECTION ( 'NONE',  ( 0.000000000000000000, 0.000000000000000000, -1.000000000000000000 ) ) ;
#2870 = CYLINDRICAL_SURFACE ( 'NONE', #18389, 4.999999999999990230 ) ;
#2871 = APPLICATION_CONTEXT ( 'automotive_design' ) ;
#2872 = VERTEX_POINT ( 'NONE', #10408 ) ;
#2873 = EDGE_LOOP ( 'NONE', ( #4370, #224, #18674, #13951 ) ) ;
#2874 = VERTEX_POINT ( 'NONE', #8943 ) ;
#2875 = EDGE_LOOP ( 'NONE', ( #10252, #12287, #87, #18860, #4916, #8454 ) ) ;
#2876 = VERTEX_POINT ( 'NONE', #2959 ) ;
#2877 = VERTEX_POINT ( 'NONE', #19859 ) ;
#2878 = CARTESIAN_POINT ( 'NONE',  ( 178.4893729001365443, 0.000000000000000000, 0.000000000000000000 ) ) ;
#2879 = CARTESIAN_POINT ( 'NONE',  ( -8.881784197001250351E-16, 17.85000000000000142, 0.000000000000000000 ) ) ;
#2880 = UNCERTAINTY_MEASURE_WITH_UNIT (LENGTH_MEASURE( 1.000000000000000082E-05 ), #3697, 'distance_accuracy_value', 'NONE');
#2881 = AXIS2_PLACEMENT_3D ( 'NONE', #17704, #9460, #3280 ) ;
#2882 = DIRECTION ( 'NONE',  ( -0.000000000000000000, 1.000000000000000000, -0.000000000000000000 ) ) ;
#2883 = SURFACE_SIDE_STYLE ('',( #9480 ) ) ;
#2884 = EDGE_CURVE ( 'NONE', #17060, #13429, #12146, .T. ) ;
#2885 =( NAMED_UNIT ( * ) PLANE_ANGLE_UNIT ( ) SI_UNIT ( $, .RADIAN. ) );
#2886 = DIRECTION ( 'NONE',  ( -0.000000000000000000, -1.000000000000000000, -0.000000000000000000 ) ) ;
#2887 =( NAMED_UNIT ( * ) PLANE_ANGLE_UNIT ( ) SI_UNIT ( $, .RADIAN. ) );
#2888 = LINE ( 'NONE', #19673, #10028 ) ;
#2889 = LINE ( 'NONE', #20094, #11273 ) ;
#2890 = CARTESIAN_POINT ( 'NONE',  ( -0.1304659433170509975, 139.6628864257297380, 500.6059509887651302 ) ) ;
#2891 = EDGE_LOOP ( 'NONE', ( #7975, #1729, #6295, #4329 ) ) ;
#2892 = DIRECTION ( 'NONE',  ( 0.000000000000000000, 0.000000000000000000, 1.000000000000000000 ) ) ;
#2893 = CARTESIAN_POINT ( 'NONE',  ( -78.99999999999995737, 142.0976792249508662, 502.3210940490797611 ) ) ;
#2894 = CARTESIAN_POINT ( 'NONE',  ( 20.99999999999996092, 0.000000000000000000, 35.00000000000000711 ) ) ;
#2895 = AXIS2_PLACEMENT_3D ( 'NONE', #3968, #8310, #14583 ) ;
#2896 = ORIENTED_EDGE ( 'NONE', *, *, #16318, .T. ) ;
#2897 = ADVANCED_FACE ( 'NONE', ( #15360 ), #14006, .F. ) ;
#2898 =( NAMED_UNIT ( * ) SI_UNIT ( $, .STERADIAN. ) SOLID_ANGLE_UNIT ( ) );
#2899 = ORIENTED_EDGE ( 'NONE', *, *, #7794, .T. ) ;
#2900 =( NAMED_UNIT ( * ) SI_UNIT ( $, .STERADIAN. ) SOLID_ANGLE_UNIT ( ) );
#2901 = VERTEX_POINT ( 'NONE', #5964 ) ;
#2902 = LINE ( 'NONE', #2704, #7758 ) ;
#2903 = CARTESIAN_POINT ( 'NONE',  ( -211.5106270998635409, 113.1299228374912502, 29.36128450348865471 ) ) ;
#2904 = LINE ( 'NONE', #13949, #15283 ) ;
#2905 =( LENGTH_UNIT ( ) NAMED_UNIT ( * ) SI_UNIT ( .MILLI., .METRE. ) );
#2906 = EDGE_CURVE ( 'NONE', #6229, #17448, #17005, .T. ) ;
#2907 = ORIENTED_EDGE ( 'NONE', *, *, #1577, .T. ) ;
#2908 = DIRECTION ( 'NONE',  ( 0.000000000000000000, 0.000000000000000000, 1.000000000000000000 ) ) ;
#2909 = ORIENTED_EDGE ( 'NONE', *, *, #12156, .F. ) ;
#2910 = SURFACE_STYLE_FILL_AREA ( #17349 ) ;
#2911 = CARTESIAN_POINT ( 'NONE',  ( 0.000000000000000000, 16.00000000000000000, 0.000000000000000000 ) ) ;
#2912 = ITEM_DEFINED_TRANSFORMATION ( 'NONE', 'NONE', #6049,  #4024 ) ;
#2913 = ORIENTED_EDGE ( 'NONE', *, *, #3858, .F. ) ;
#2914 = PRODUCT_DEFINITION ( 'UNKNOWN', '', #13905, #18103 ) ;
#2915 = CARTESIAN_POINT ( 'NONE',  ( 498.8117674897343932, 134.2156642432025251, -87.31255586191144857 ) ) ;
#2916 = ORIENTED_EDGE ( 'NONE', *, *, #1935, .T. ) ;
#2917 = EDGE_LOOP ( 'NONE', ( #10835, #9546, #6909, #15411 ) ) ;
#2918 = AXIS2_PLACEMENT_3D ( 'NONE', #15600, #19344, #15490 ) ;
#2919 = AXIS2_PLACEMENT_3D ( 'NONE', #13074, #13369, #14883 ) ;
#2920 = VERTEX_POINT ( 'NONE', #9250 ) ;
#2921 = EDGE_CURVE ( 'NONE', #693, #19038, #1091, .T. ) ;
#2922 = LINE ( 'NONE', #13757, #6794 ) ;
#2923 = ORIENTED_EDGE ( 'NONE', *, *, #7535, .T. ) ;
#2924 = ADVANCED_FACE ( 'NONE', ( #15247 ), #16902, .F. ) ;
#2925 = DIRECTION ( 'NONE',  ( -1.000000000000000000, 0.000000000000000000, 0.000000000000000000 ) ) ;
#2926 = ORIENTED_EDGE ( 'NONE', *, *, #3753, .F. ) ;
#2927 = CARTESIAN_POINT ( 'NONE',  ( -23.00000000000002487, 6.000000000000000000, -36.99999999999999289 ) ) ;
#2928 = CARTESIAN_POINT ( 'NONE',  ( -18.00000000000001421, 6.000000000000000000, 37.00000000000000711 ) ) ;
#2929 = CARTESIAN_POINT ( 'NONE',  ( 463.8334540492693350, 191.8198460455371333, 178.2339398819846110 ) ) ;
#2930 =( GEOMETRIC_REPRESENTATION_CONTEXT ( 3 ) GLOBAL_UNCERTAINTY_ASSIGNED_CONTEXT ( ( #2049 ) ) GLOBAL_UNIT_ASSIGNED_CONTEXT ( ( #5162, #11741, #3901 ) ) REPRESENTATION_CONTEXT ( 'NONE', 'WORKASPACE' ) );
#2931 = CARTESIAN_POINT ( 'NONE',  ( 133.4893729001365443, 123.1299228374914634, 29.36128450348865471 ) ) ;
#2933 = EDGE_CURVE ( 'NONE', #6958, #1468, #10494, .T. ) ;
#2932 = DIRECTION ( 'NONE',  ( -5.889072920838430686E-16, 1.000000000000000000, -0.000000000000000000 ) ) ;
#2934 = CARTESIAN_POINT ( 'NONE',  ( 10.00000000000000000, 376.0487089519837127, -150.0000000000033538 ) ) ;
#2935 = ADVANCED_FACE ( 'NONE', ( #16796 ), #18325, .F. ) ;
#2936 = CIRCLE ( 'NONE', #13494, 3.283624802691453848 ) ;
#2937 = SURFACE_STYLE_FILL_AREA ( #12217 ) ;
#2938 = DIRECTION ( 'NONE',  ( -1.000000000000000000, 0.000000000000000000, 7.715811803773179210E-14 ) ) ;
#2939 =( LENGTH_UNIT ( ) NAMED_UNIT ( * ) SI_UNIT ( .MILLI., .METRE. ) );
#2940 = LINE ( 'NONE', #10579, #4051 ) ;
#2941 = CARTESIAN_POINT ( 'NONE',  ( 3.000000000000000000, 1.836909530733570325E-16, 3.000000000000000000 ) ) ;
#2942 = DIRECTION ( 'NONE',  ( 0.000000000000000000, 1.000000000000000000, -0.000000000000000000 ) ) ;
#2943 = EDGE_CURVE ( 'NONE', #13434, #4175, #13705, .T. ) ;
#2944 = CARTESIAN_POINT ( 'NONE',  ( -0.6359441111628246768, 138.8819879824800125, 489.5547513090041889 ) ) ;
#2945 = CYLINDRICAL_SURFACE ( 'NONE', #2948, 2.000000000000001776 ) ;
#2946 = ORIENTED_EDGE ( 'NONE', *, *, #7339, .T. ) ;
#2947 = EDGE_CURVE ( 'NONE', #3192, #17522, #14703, .T. ) ;
#2948 = AXIS2_PLACEMENT_3D ( 'NONE', #8214, #466, #11500 ) ;
#2949 = ADVANCED_FACE ( 'NONE', ( #20057 ), #12242, .F. ) ;
#2950 = ORIENTED_EDGE ( 'NONE', *, *, #8859, .T. ) ;
#2951 = AXIS2_PLACEMENT_3D ( 'NONE', #14995, #7556, #16943 ) ;
#2952 = ORIENTED_EDGE ( 'NONE', *, *, #2053, .F. ) ;
#2953 = CARTESIAN_POINT ( 'NONE',  ( 43.00000000000001421, 0.000000000000000000, 0.000000000000000000 ) ) ;
#2954 = ADVANCED_FACE ( 'NONE', ( #1909 ), #11109, .T. ) ;
#2955 = ORIENTED_EDGE ( 'NONE', *, *, #2998, .F. ) ;
#2956 = DIRECTION ( 'NONE',  ( 0.000000000000000000, 0.000000000000000000, -1.000000000000000000 ) ) ;
#2957 = DIRECTION ( 'NONE',  ( 0.000000000000000000, 1.000000000000000000, 0.000000000000000000 ) ) ;
#2958 = EDGE_LOOP ( 'NONE', ( #5308, #618 ) ) ;
#2959 = CARTESIAN_POINT ( 'NONE',  ( 153.4893729001366864, 103.1299228374914492, 170.4174721992565082 ) ) ;
#2960 = DIRECTION ( 'NONE',  ( 1.000000000000000000, -0.000000000000000000, -0.000000000000000000 ) ) ;
#2961 = EDGE_CURVE ( 'NONE', #2483, #1058, #7980, .T. ) ;
#2962 = FILL_AREA_STYLE ('',( #20278 ) ) ;
#2963 = DIRECTION ( 'NONE',  ( 0.000000000000000000, 0.000000000000000000, 1.000000000000000000 ) ) ;
#2964 = CARTESIAN_POINT ( 'NONE',  ( -32.00000000000000711, 6.000000000000000000, -22.00000000000000355 ) ) ;
#2965 = DIRECTION ( 'NONE',  ( 1.000000000000000000, 0.000000000000000000, 0.000000000000000000 ) ) ;
#2966 = VECTOR ( 'NONE', #8079, 1000.000000000000000 ) ;
#2967 = AXIS2_PLACEMENT_3D ( 'NONE', #4443, #10730, #17024 ) ;
#2968 = DIRECTION ( 'NONE',  ( 0.000000000000000000, 0.000000000000000000, 1.000000000000000000 ) ) ;
#2969 = CARTESIAN_POINT ( 'NONE',  ( 37.00000000000000000, 68.00000000000000000, 23.00000000000001066 ) ) ;
#2970 = COLOUR_RGB ( '', 0.40784314, 0.44705882, 0.49803922) ;
#2971 = EDGE_CURVE ( 'NONE', #198, #20118, #3278, .T. ) ;
#2972 = EDGE_LOOP ( 'NONE', ( #13779, #16068, #17879, #15607, #15778, #14983 ) ) ;
#2973 = VERTEX_POINT ( 'NONE', #19132 ) ;
#2974 = ORIENTED_EDGE ( 'NONE', *, *, #9373, .F. ) ;
#2975 = EDGE_CURVE ( 'NONE', #4114, #14513, #185, .T. ) ;
#2976 = CARTESIAN_POINT ( 'NONE',  ( 133.4893729001365728, 80.91625508013694912, -97.94896630388704750 ) ) ;
#2977 = EDGE_LOOP ( 'NONE', ( #9265, #3920 ) ) ;
#2978 = ORIENTED_EDGE ( 'NONE', *, *, #14416, .F. ) ;
#2979 = ORIENTED_EDGE ( 'NONE', *, *, #8936, .T. ) ;
#2980 = CARTESIAN_POINT ( 'NONE',  ( -23.00000000000002132, 10.00000000000000000, 37.00000000000000711 ) ) ;
#2981 = AXIS2_PLACEMENT_3D ( 'NONE', #10858, #15623, #15516 ) ;
#2982 = EDGE_CURVE ( 'NONE', #865, #12374, #74, .T. ) ;
#2983 = AXIS2_PLACEMENT_3D ( 'NONE', #4776, #11056, #17334 ) ;
#2984 = SURFACE_STYLE_USAGE ( .BOTH. , #17103 ) ;
#2985 = LINE ( 'NONE', #10428, #10912 ) ;
#2986 = DIRECTION ( 'NONE',  ( -0.000000000000000000, -1.000000000000000000, -0.000000000000000000 ) ) ;
#2987 = ORIENTED_EDGE ( 'NONE', *, *, #18220, .T. ) ;
#2988 =( LENGTH_UNIT ( ) NAMED_UNIT ( * ) SI_UNIT ( .MILLI., .METRE. ) );
#2989 = DIRECTION ( 'NONE',  ( 1.000000000000000000, 0.000000000000000000, 0.000000000000000000 ) ) ;
#2990 =( NAMED_UNIT ( * ) PLANE_ANGLE_UNIT ( ) SI_UNIT ( $, .RADIAN. ) );
#2991 = CARTESIAN_POINT ( 'NONE',  ( 463.8334540492693350, 214.2156642432025251, 250.0000000000000000 ) ) ;
#2992 = EDGE_LOOP ( 'NONE', ( #15930, #11221, #8173, #11413 ) ) ;
#2993 = LINE ( 'NONE', #13929, #5898 ) ;
#2994 =( GEOMETRIC_REPRESENTATION_CONTEXT ( 3 ) GLOBAL_UNCERTAINTY_ASSIGNED_CONTEXT ( ( #16333 ) ) GLOBAL_UNIT_ASSIGNED_CONTEXT ( ( #6563, #17574, #16064 ) ) REPRESENTATION_CONTEXT ( 'NONE', 'WORKASPACE' ) );
#2995 = DIRECTION ( 'NONE',  ( 1.000000000000000000, 0.000000000000000000, -0.000000000000000000 ) ) ;
#2996 = AXIS2_PLACEMENT_3D ( 'NONE', #8527, #19637, #9878 ) ;
#2997 = STYLED_ITEM ( 'NONE', ( #3096 ), #7742 ) ;
#2998 = EDGE_CURVE ( 'NONE', #3066, #10187, #18823, .T. ) ;
#2999 = ORIENTED_EDGE ( 'NONE', *, *, #17055, .T. ) ;
#3000 = FILL_AREA_STYLE_COLOUR ( '', #8087 ) ;
#3001 = ORIENTED_EDGE ( 'NONE', *, *, #8591, .F. ) ;
#3002 = FILL_AREA_STYLE ('',( #3316 ) ) ;
#3003 = VECTOR ( 'NONE', #16589, 1000.000000000000000 ) ;
#3004 = DIRECTION ( 'NONE',  ( 5.099857904826348903E-14, -0.3949357872488050702, -0.9187087263927378178 ) ) ;
#3005 = ORIENTED_EDGE ( 'NONE', *, *, #17121, .F. ) ;
#3006 = DIRECTION ( 'NONE',  ( -0.000000000000000000, 1.000000000000000000, -0.000000000000000000 ) ) ;
#3007 = DIRECTION ( 'NONE',  ( -0.000000000000000000, -1.000000000000000000, -0.000000000000000000 ) ) ;
#3008 = SURFACE_SIDE_STYLE ('',( #3320 ) ) ;
#3009 = VECTOR ( 'NONE', #8827, 1000.000000000000000 ) ;
#3010 = CARTESIAN_POINT ( 'NONE',  ( 0.6373225965090424383, 139.7798076373073286, 500.8838725201990769 ) ) ;
#3011 = DIRECTION ( 'NONE',  ( 1.000000000000000000, 5.889072920838430686E-16, 0.000000000000000000 ) ) ;
#3012 = CARTESIAN_POINT ( 'NONE',  ( 31.00000000000003908, 19.00000000000000000, -26.00000000000000355 ) ) ;
#3013 = DIRECTION ( 'NONE',  ( 1.000000000000000000, 5.889072920838430686E-16, -0.000000000000000000 ) ) ;
#3014 = VERTEX_POINT ( 'NONE', #17184 ) ;
#3015 = SURFACE_SIDE_STYLE ('',( #9510 ) ) ;
#3016 = DIRECTION ( 'NONE',  ( -0.000000000000000000, 0.000000000000000000, -1.000000000000000000 ) ) ;
#3017 = PRODUCT_CONTEXT ( 'NONE', #15534, 'mechanical' ) ;
#3018 = ORIENTED_EDGE ( 'NONE', *, *, #11519, .F. ) ;
#3019 = CARTESIAN_POINT ( 'NONE',  ( 18.99999999999998224, 8.000000000000000000, -35.99999999999999289 ) ) ;
#3020 = ORIENTED_EDGE ( 'NONE', *, *, #11532, .T. ) ;
#3021 = VECTOR ( 'NONE', #10865, 1000.000000000000000 ) ;
#3022 = ORIENTED_EDGE ( 'NONE', *, *, #1404, .F. ) ;
#3023 = EDGE_CURVE ( 'NONE', #17862, #506, #8229, .T. ) ;
#3024 =( GEOMETRIC_REPRESENTATION_CONTEXT ( 3 ) GLOBAL_UNCERTAINTY_ASSIGNED_CONTEXT ( ( #10539 ) ) GLOBAL_UNIT_ASSIGNED_CONTEXT ( ( #2320, #16472, #9772 ) ) REPRESENTATION_CONTEXT ( 'NONE', 'WORKASPACE' ) );
#3025 = ORIENTED_EDGE ( 'NONE', *, *, #19595, .F. ) ;
#3026 = LINE ( 'NONE', #6450, #1815 ) ;
#3027 = AXIS2_PLACEMENT_3D ( 'NONE', #9970, #16386, #13390 ) ;
#3028 = ORIENTED_EDGE ( 'NONE', *, *, #5988, .F. ) ;
#3029 = CARTESIAN_POINT ( 'NONE',  ( 37.00000000000003553, -20.00000000000000000, 20.00000000000000000 ) ) ;
#3030 = DIRECTION ( 'NONE',  ( -0.000000000000000000, -0.000000000000000000, 1.000000000000000000 ) ) ;
#3031 = SURFACE_STYLE_USAGE ( .BOTH. , #15644 ) ;
#3032 = VECTOR ( 'NONE', #8028, 1000.000000000000000 ) ;
#3033 = VECTOR ( 'NONE', #15958, 1000.000000000000000 ) ;
#3034 = DIRECTION ( 'NONE',  ( -0.000000000000000000, -1.000000000000000000, -0.000000000000000000 ) ) ;
#3035 = CARTESIAN_POINT ( 'NONE',  ( 463.8334540492693350, 191.8198460455371333, 24.99421986894476078 ) ) ;
#3036 =( GEOMETRIC_REPRESENTATION_CONTEXT ( 3 ) GLOBAL_UNCERTAINTY_ASSIGNED_CONTEXT ( ( #12890 ) ) GLOBAL_UNIT_ASSIGNED_CONTEXT ( ( #19405, #10145, #14380 ) ) REPRESENTATION_CONTEXT ( 'NONE', 'WORKASPACE' ) );
#3037 = EDGE_LOOP ( 'NONE', ( #5651, #1146, #2823, #20124 ) ) ;
#3038 = DIRECTION ( 'NONE',  ( 0.000000000000000000, 0.000000000000000000, -1.000000000000000000 ) ) ;
#3039 = EDGE_CURVE ( 'NONE', #9147, #20015, #15768, .T. ) ;
#3040 =( NAMED_UNIT ( * ) PLANE_ANGLE_UNIT ( ) SI_UNIT ( $, .RADIAN. ) );
#3041 = DIRECTION ( 'NONE',  ( 0.000000000000000000, 1.000000000000000000, -0.000000000000000000 ) ) ;
#3042 = DIRECTION ( 'NONE',  ( -0.000000000000000000, -1.000000000000000000, -0.000000000000000000 ) ) ;
#3043 = LINE ( 'NONE', #1582, #12592 ) ;
#3044 = PRODUCT_DEFINITION_FORMATION_WITH_SPECIFIED_SOURCE ( 'ANY', '', #11412, .NOT_KNOWN. ) ;
#3045 = VECTOR ( 'NONE', #6458, 1000.000000000000000 ) ;
#3046 =( NAMED_UNIT ( * ) SI_UNIT ( $, .STERADIAN. ) SOLID_ANGLE_UNIT ( ) );
#3047 = VECTOR ( 'NONE', #7244, 1000.000000000000000 ) ;
#3048 = ORIENTED_EDGE ( 'NONE', *, *, #4890, .T. ) ;
#3049 = VERTEX_POINT ( 'NONE', #15868 ) ;
#3050 = VECTOR ( 'NONE', #6748, 1000.000000000000000 ) ;
#3051 = ORIENTED_EDGE ( 'NONE', *, *, #16596, .F. ) ;
#3052 = EDGE_CURVE ( 'NONE', #4741, #8486, #8021, .T. ) ;
#3053 = ORIENTED_EDGE ( 'NONE', *, *, #15093, .F. ) ;
#3054 = PRESENTATION_STYLE_ASSIGNMENT (( #11199 ) ) ;
#3055 = CARTESIAN_POINT ( 'NONE',  ( -81.00000000000260059, 138.7723821175108014, 490.5025619657601510 ) ) ;
#3056 = ORIENTED_EDGE ( 'NONE', *, *, #13892, .F. ) ;
#3057 = FILL_AREA_STYLE_COLOUR ( '', #7409 ) ;
#3058 = SURFACE_STYLE_USAGE ( .BOTH. , #14003 ) ;
#3059 = CLOSED_SHELL ( 'NONE', ( #18447, #928, #20320, #10717, #8779, #8754, #15066, #5130, #6368, #3983, #9657, #14385, #5391, #8871, #5049, #19052, #1989, #20356, #19608, #8191, #8910, #5619, #1438, #19980, #13072, #17282, #1406, #10318, #9286, #10016, #4634, #18146, #12057, #6807, #8881, #19, #6662, #3883, #13305, #6113, #19304, #10011, #14678, #6749, #11784, #14480, #16891, #15441, #15741, #19013, #15945, #6705, #628, #9238, #8277, #216, #277, #7549, #19929, #15148, #14086, #2954, #10171, #7440, #5473, #558 ) ) ;
#3060 = ADVANCED_FACE ( 'NONE', ( #14304 ), #17295, .T. ) ;
#3061 = VECTOR ( 'NONE', #12880, 1000.000000000000000 ) ;
#3062 = EDGE_LOOP ( 'NONE', ( #6024, #11843 ) ) ;
#3063 = SURFACE_STYLE_FILL_AREA ( #7717 ) ;
#3064 = SURFACE_STYLE_USAGE ( .BOTH. , #12772 ) ;
#3065 = DIRECTION ( 'NONE',  ( 0.000000000000000000, 0.000000000000000000, 1.000000000000000000 ) ) ;
#3066 = VERTEX_POINT ( 'NONE', #3495 ) ;
#3067 = CARTESIAN_POINT ( 'NONE',  ( -3.000000000000002220, 60.19966235751221006, 9.013878188659974811 ) ) ;
#3068 = CARTESIAN_POINT ( 'NONE',  ( 463.8334540492693350, 191.8198460455371333, 91.76606011801541740 ) ) ;
#3069 = AXIS2_PLACEMENT_3D ( 'NONE', #8875, #13618, #18346 ) ;
#3070 = CIRCLE ( 'NONE', #14594, 34.00000000000000000 ) ;
#3071 = DIRECTION ( 'NONE',  ( -0.000000000000000000, -1.000000000000000000, -0.000000000000000000 ) ) ;
#3072 = DIRECTION ( 'NONE',  ( -1.000000000000000000, -0.000000000000000000, -0.000000000000000000 ) ) ;
#3073 = ADVANCED_FACE ( 'NONE', ( #12876 ), #11423, .F. ) ;
#3074 = FACE_OUTER_BOUND ( 'NONE', #6651, .T. ) ;
#3075 = ORIENTED_EDGE ( 'NONE', *, *, #10003, .F. ) ;
#3076 = LINE ( 'NONE', #6594, #4315 ) ;
#3077 = DIRECTION ( 'NONE',  ( -3.854941057726249437E-16, 0.000000000000000000, -1.000000000000000000 ) ) ;
#3078 = EDGE_CURVE ( 'NONE', #17763, #6154, #19629, .T. ) ;
#3079 =( GEOMETRIC_REPRESENTATION_CONTEXT ( 3 ) GLOBAL_UNCERTAINTY_ASSIGNED_CONTEXT ( ( #14877 ) ) GLOBAL_UNIT_ASSIGNED_CONTEXT ( ( #14476, #5215, #2289 ) ) REPRESENTATION_CONTEXT ( 'NONE', 'WORKASPACE' ) );
#3080 = VECTOR ( 'NONE', #1731, 1000.000000000000000 ) ;
#3081 = ORIENTED_EDGE ( 'NONE', *, *, #18666, .T. ) ;
#3082 = ORIENTED_EDGE ( 'NONE', *, *, #7846, .F. ) ;
#3083 = ORIENTED_EDGE ( 'NONE', *, *, #6477, .F. ) ;
#3084 = EDGE_CURVE ( 'NONE', #12290, #8120, #5536, .T. ) ;
#3085 = ORIENTED_EDGE ( 'NONE', *, *, #3129, .F. ) ;
#3086 = EDGE_LOOP ( 'NONE', ( #1799, #11503, #11577, #5397, #8148 ) ) ;
#3087 = CIRCLE ( 'NONE', #8024, 10.00000000000000888 ) ;
#3088 = AXIS2_PLACEMENT_3D ( 'NONE', #15624, #3016, #18880 ) ;
#3089 = VERTEX_POINT ( 'NONE', #17998 ) ;
#3090 = DIRECTION ( 'NONE',  ( 0.000000000000000000, 0.000000000000000000, -1.000000000000000000 ) ) ;
#3091 = COLOUR_RGB ( '', 0.66274510, 0.83137255, 0.94901961) ;
#3092 = PRESENTATION_LAYER_ASSIGNMENT (  '', '', ( #5730 ) ) ;
#3093 = VERTEX_POINT ( 'NONE', #2128 ) ;
#3094 = CARTESIAN_POINT ( 'NONE',  ( -81.00000000000260059, 138.7723821175108014, 490.5025619657601510 ) ) ;
#3095 = STYLED_ITEM ( 'NONE', ( #165 ), #15540 ) ;
#3096 = PRESENTATION_STYLE_ASSIGNMENT (( #3200 ) ) ;
#3097 =( NAMED_UNIT ( * ) PLANE_ANGLE_UNIT ( ) SI_UNIT ( $, .RADIAN. ) );
#3098 = LINE ( 'NONE', #12270, #15690 ) ;
#3099 = ADVANCED_FACE ( 'NONE', ( #2324 ), #11730, .F. ) ;
#3100 = AXIS2_PLACEMENT_3D ( 'NONE', #13943, #3126, #15721 ) ;
#3101 = DIRECTION ( 'NONE',  ( 0.000000000000000000, 0.000000000000000000, -1.000000000000000000 ) ) ;
#3102 = LINE ( 'NONE', #4758, #12624 ) ;
#3103 = VECTOR ( 'NONE', #9244, 1000.000000000000000 ) ;
#3104 = CARTESIAN_POINT ( 'NONE',  ( -39.99999999999997868, -20.00000000000000000, -19.99999999999999645 ) ) ;
#3105 = ADVANCED_FACE ( 'NONE', ( #5150 ), #11826, .T. ) ;
#3106 = LINE ( 'NONE', #17112, #17206 ) ;
#3107 = CARTESIAN_POINT ( 'NONE',  ( -1.000000000000012657, 140.8764026050585869, 502.4686618848270996 ) ) ;
#3108 = ORIENTED_EDGE ( 'NONE', *, *, #19912, .F. ) ;
#3109 = LINE ( 'NONE', #14126, #19553 ) ;
#3110 = COLOUR_RGB ( '', 0.08235294, 0.09019608, 0.10196078) ;
#3111 = VECTOR ( 'NONE', #2042, 1000.000000000000000 ) ;
#3112 = CARTESIAN_POINT ( 'NONE',  ( 31.99999999999998579, 10.00000000000000000, 21.99999999999999645 ) ) ;
#3113 = VECTOR ( 'NONE', #4765, 1000.000000000000000 ) ;
#3114 = CIRCLE ( 'NONE', #2116, 8.999999999999952038 ) ;
#3115 = CIRCLE ( 'NONE', #13976, 3.000000000000002665 ) ;
#3116 = EDGE_LOOP ( 'NONE', ( #11356, #4558, #507, #1924 ) ) ;
#3117 = PRESENTATION_LAYER_ASSIGNMENT (  '', '', ( #6088 ) ) ;
#3118 = DIRECTION ( 'NONE',  ( 0.000000000000000000, 1.000000000000000000, 0.000000000000000000 ) ) ;
#3119 = ORIENTED_EDGE ( 'NONE', *, *, #19651, .F. ) ;
#3120 = EDGE_CURVE ( 'NONE', #11214, #12937, #10268, .T. ) ;
#3121 = MECHANICAL_DESIGN_GEOMETRIC_PRESENTATION_REPRESENTATION (  '', ( #14320 ), #10681 ) ;
#3122 =( LENGTH_UNIT ( ) NAMED_UNIT ( * ) SI_UNIT ( .MILLI., .METRE. ) );
#3123 = LINE ( 'NONE', #15718, #15147 ) ;
#3124 = COLOUR_RGB ( '', 0.08235294, 0.09019608, 0.10196078) ;
#3125 = ORIENTED_EDGE ( 'NONE', *, *, #19252, .T. ) ;
#3126 = DIRECTION ( 'NONE',  ( -9.815121534730717399E-17, 1.000000000000000000, -2.352167425053297897E-16 ) ) ;
#3127 = CIRCLE ( 'NONE', #14992, 18.50000000000000000 ) ;
#3128 = DIRECTION ( 'NONE',  ( -1.000000000000000000, 0.000000000000000000, 0.000000000000000000 ) ) ;
#3129 = EDGE_CURVE ( 'NONE', #6137, #6221, #8958, .T. ) ;
#3130 = ADVANCED_FACE ( 'NONE', ( #2220 ), #15020, .F. ) ;
#3131 = CARTESIAN_POINT ( 'NONE',  ( 1.181929469892549101, 147.7545334744432921, 491.0690926367356042 ) ) ;
#3132 = LINE ( 'NONE', #15724, #15078 ) ;
#3133 = LINE ( 'NONE', #12725, #8904 ) ;
#3134 = CARTESIAN_POINT ( 'NONE',  ( 31.00000000000000000, 19.00000000000000000, -31.00000000000000355 ) ) ;
#3135 = AXIS2_PLACEMENT_3D ( 'NONE', #2834, #4093, #961 ) ;
#3136 = EDGE_LOOP ( 'NONE', ( #10951, #16764, #3766, #2003 ) ) ;
#3137 = DIRECTION ( 'NONE',  ( 1.322948291343117631E-12, 0.000000000000000000, 1.000000000000000000 ) ) ;
#3138 = CARTESIAN_POINT ( 'NONE',  ( 0.000000000000000000, 66.00000000000000000, -5.741599279633704455E-16 ) ) ;
#3139 = PLANE ( 'NONE',  #15282 ) ;
#3140 = CONTEXT_DEPENDENT_SHAPE_REPRESENTATION ( #1004, #5952 ) ;
#3141 = AXIS2_PLACEMENT_3D ( 'NONE', #15361, #10495, #1189 ) ;
#3142 = ORIENTED_EDGE ( 'NONE', *, *, #19807, .T. ) ;
#3143 = EDGE_LOOP ( 'NONE', ( #9080, #12138, #14871, #7231 ) ) ;
#3144 = DIRECTION ( 'NONE',  ( -0.000000000000000000, 0.000000000000000000, 1.000000000000000000 ) ) ;
#3145 = VERTEX_POINT ( 'NONE', #14915 ) ;
#3146 = VERTEX_POINT ( 'NONE', #14716 ) ;
#3147 = VECTOR ( 'NONE', #13155, 1000.000000000000000 ) ;
#3148 = VERTEX_POINT ( 'NONE', #586 ) ;
#3149 = VECTOR ( 'NONE', #3539, 1000.000000000000000 ) ;
#3150 = DIRECTION ( 'NONE',  ( -0.000000000000000000, -1.000000000000000000, 0.000000000000000000 ) ) ;
#3151 = ORIENTED_EDGE ( 'NONE', *, *, #14163, .F. ) ;
#3152 = FACE_BOUND ( 'NONE', #18412, .T. ) ;
#3153 = EDGE_LOOP ( 'NONE', ( #1346, #11323, #9713, #9987 ) ) ;
#3154 = LINE ( 'NONE', #2927, #1405 ) ;
#3155 = DIRECTION ( 'NONE',  ( -0.000000000000000000, 1.000000000000000000, -0.000000000000000000 ) ) ;
#3156 =( REPRESENTATION_RELATIONSHIP ('NONE','NONE', #12483, #16721 ) REPRESENTATION_RELATIONSHIP_WITH_TRANSFORMATION ( #13956 )SHAPE_REPRESENTATION_RELATIONSHIP( ) );
#3157 = LINE ( 'NONE', #153, #10874 ) ;
#3158 = DIRECTION ( 'NONE',  ( 0.000000000000000000, 1.000000000000000000, 0.000000000000000000 ) ) ;
#3159 = EDGE_CURVE ( 'NONE', #9451, #3146, #13183, .T. ) ;
#3160 = DIRECTION ( 'NONE',  ( 0.000000000000000000, 0.000000000000000000, 1.000000000000000000 ) ) ;
#3161 = ORIENTED_EDGE ( 'NONE', *, *, #18151, .T. ) ;
#3162 = DIRECTION ( 'NONE',  ( 1.000000000000000000, 0.000000000000000000, -0.000000000000000000 ) ) ;
#3163 = FACE_OUTER_BOUND ( 'NONE', #6625, .T. ) ;
#3164 = DIRECTION ( 'NONE',  ( 0.000000000000000000, 1.000000000000000000, 0.000000000000000000 ) ) ;
#3165 = FILL_AREA_STYLE_COLOUR ( '', #9019 ) ;
#3166 = DIRECTION ( 'NONE',  ( 0.000000000000000000, 1.000000000000000000, 0.000000000000000000 ) ) ;
#3167 = CIRCLE ( 'NONE', #4470, 10.00000000000001066 ) ;
#3168 = EDGE_LOOP ( 'NONE', ( #16914, #2978, #2298, #17710 ) ) ;
#3169 = PRODUCT ( 'Servo-Body.2', 'Servo-Body.2', '', ( #12612 ) ) ;
#3170 = VERTEX_POINT ( 'NONE', #8333 ) ;
#3171 =( NAMED_UNIT ( * ) PLANE_ANGLE_UNIT ( ) SI_UNIT ( $, .RADIAN. ) );
#3172 = CARTESIAN_POINT ( 'NONE',  ( -79.99999999999995737, 141.6406393683236900, 501.8237260975784011 ) ) ;
#3173 = EDGE_CURVE ( 'NONE', #18128, #14376, #777, .T. ) ;
#3174 = ORIENTED_EDGE ( 'NONE', *, *, #13775, .F. ) ;
#3175 = VECTOR ( 'NONE', #13887, 1000.000000000000000 ) ;
#3176 = CARTESIAN_POINT ( 'NONE',  ( -26.00000000000002132, 10.00000000000000000, -39.99999999999999289 ) ) ;
#3177 =( NAMED_UNIT ( * ) PLANE_ANGLE_UNIT ( ) SI_UNIT ( $, .RADIAN. ) );
#3178 = VERTEX_POINT ( 'NONE', #3688 ) ;
#3179 = COLOUR_RGB ( '', 0.31764706, 0.68627451, 0.89019608) ;
#3180 = SURFACE_STYLE_FILL_AREA ( #6481 ) ;
#3181 = DIRECTION ( 'NONE',  ( -0.000000000000000000, 1.000000000000000000, -0.000000000000000000 ) ) ;
#3182 = LINE ( 'NONE', #15771, #11311 ) ;
#3183 = CARTESIAN_POINT ( 'NONE',  ( 0.000000000000000000, 309.2289037985885898, -83.18019484660915452 ) ) ;
#3184 = DIRECTION ( 'NONE',  ( 0.000000000000000000, 0.000000000000000000, 1.000000000000000000 ) ) ;
#3185 = CARTESIAN_POINT ( 'NONE',  ( 3.500000000000000000, 0.000000000000000000, 0.000000000000000000 ) ) ;
#3186 = CARTESIAN_POINT ( 'NONE',  ( 111.4893729001366012, 122.8810204491430369, 280.0825295754780768 ) ) ;
#3187 = EDGE_CURVE ( 'NONE', #5210, #18534, #16882, .T. ) ;
#3188 = CARTESIAN_POINT ( 'NONE',  ( -22.00000000000001776, 10.00000000000000000, 32.00000000000000711 ) ) ;
#3189 = CARTESIAN_POINT ( 'NONE',  ( 0.000000000000000000, 301.0487089519837127, -150.0000000000038369 ) ) ;
#3190 = ADVANCED_FACE ( 'NONE', ( #14807 ), #7101, .F. ) ;
#3191 = ORIENTED_EDGE ( 'NONE', *, *, #1162, .F. ) ;
#3192 = VERTEX_POINT ( 'NONE', #16576 ) ;
#3193 = UNCERTAINTY_MEASURE_WITH_UNIT (LENGTH_MEASURE( 1.000000000000000082E-05 ), #8681, 'distance_accuracy_value', 'NONE');
#3194 = FILL_AREA_STYLE ('',( #1298 ) ) ;
#3195 = ORIENTED_EDGE ( 'NONE', *, *, #4304, .F. ) ;
#3196 = VERTEX_POINT ( 'NONE', #2431 ) ;
#3197 = VERTEX_POINT ( 'NONE', #8737 ) ;
#3198 = CARTESIAN_POINT ( 'NONE',  ( -39.99999999999999289, 11.00000000000000000, -34.99999999999997868 ) ) ;
#3199 = CARTESIAN_POINT ( 'NONE',  ( 178.4893729001365443, 167.9162550801369491, -97.94896630388704750 ) ) ;
#3200 = SURFACE_STYLE_USAGE ( .BOTH. , #19041 ) ;
#3201 = EDGE_CURVE ( 'NONE', #6154, #19577, #7194, .T. ) ;
#3202 = FILL_AREA_STYLE_COLOUR ( '', #13519 ) ;
#3203 = DIRECTION ( 'NONE',  ( 0.000000000000000000, 0.000000000000000000, -1.000000000000000000 ) ) ;
#3204 = DIRECTION ( 'NONE',  ( -1.000000000000000000, 0.000000000000000000, 0.000000000000000000 ) ) ;
#3205 = VECTOR ( 'NONE', #14949, 1000.000000000000000 ) ;
#3206 = CARTESIAN_POINT ( 'NONE',  ( -20.00000000000003197, 3.000000000000000000, 40.00000000000000711 ) ) ;
#3207 = EDGE_CURVE ( 'NONE', #12943, #11965, #678, .T. ) ;
#3208 = VERTEX_POINT ( 'NONE', #6990 ) ;
#3209 = DIRECTION ( 'NONE',  ( 7.715811803773179210E-14, 0.000000000000000000, 1.000000000000000000 ) ) ;
#3210 = DIRECTION ( 'NONE',  ( 0.000000000000000000, 0.000000000000000000, -1.000000000000000000 ) ) ;
#3211 = EDGE_CURVE ( 'NONE', #1495, #11244, #1694, .T. ) ;
#3212 = PRESENTATION_LAYER_ASSIGNMENT (  '', '', ( #12101 ) ) ;
#3213 = EDGE_CURVE ( 'NONE', #11216, #6215, #18159, .T. ) ;
#3214 = AXIS2_PLACEMENT_3D ( 'NONE', #20279, #9364, #12462 ) ;
#3215 = ORIENTED_EDGE ( 'NONE', *, *, #14800, .T. ) ;
#3216 = EDGE_CURVE ( 'NONE', #10863, #5026, #7001, .T. ) ;
#3217 = LINE ( 'NONE', #8174, #8573 ) ;
#3218 = EDGE_LOOP ( 'NONE', ( #12689, #4803, #13144, #14286 ) ) ;
#3219 = EDGE_CURVE ( 'NONE', #5436, #1247, #13479, .T. ) ;
#3220 = DIRECTION ( 'NONE',  ( 0.000000000000000000, 0.7699350945217658948, 0.6381222063396316813 ) ) ;
#3221 = CARTESIAN_POINT ( 'NONE',  ( 31.00000000000006395, 68.00000000000000000, -22.99999999999999289 ) ) ;
#3222 = ORIENTED_EDGE ( 'NONE', *, *, #7227, .T. ) ;
#3223 = DIRECTION ( 'NONE',  ( 1.000000000000000000, -0.000000000000000000, 0.000000000000000000 ) ) ;
#3224 = LINE ( 'NONE', #1330, #4405 ) ;
#3225 =( NAMED_UNIT ( * ) SI_UNIT ( $, .STERADIAN. ) SOLID_ANGLE_UNIT ( ) );
#3226 = CARTESIAN_POINT ( 'NONE',  ( 0.1799495709128176857, 139.9667223049720235, 501.2039705546205823 ) ) ;
#3227 = DIRECTION ( 'NONE',  ( -0.000000000000000000, -1.000000000000000000, -0.000000000000000000 ) ) ;
#3228 = DIRECTION ( 'NONE',  ( -0.000000000000000000, -1.000000000000000000, -0.000000000000000000 ) ) ;
#3229 = CARTESIAN_POINT ( 'NONE',  ( -38.50085094405407204, 209.4098724938429541, 505.3921618609452935 ) ) ;
#3230 = ORIENTED_EDGE ( 'NONE', *, *, #20156, .T. ) ;
#3231 = DIRECTION ( 'NONE',  ( 0.000000000000000000, 0.000000000000000000, -1.000000000000000000 ) ) ;
#3232 = CARTESIAN_POINT ( 'NONE',  ( 53.48937290013659407, 209.4935875941501422, 345.2279431939882670 ) ) ;
#3233 = CARTESIAN_POINT ( 'NONE',  ( -22.00000000000001776, 6.000000000000000000, 32.00000000000000711 ) ) ;
#3234 = APPLICATION_PROTOCOL_DEFINITION ( 'draft international standard', 'automotive_design', 1998, #10521 ) ;
#3235 = VERTEX_POINT ( 'NONE', #8832 ) ;
#3236 = VERTEX_POINT ( 'NONE', #18610 ) ;
#3237 = DIRECTION ( 'NONE',  ( 1.000000000000000000, 0.000000000000000000, 0.000000000000000000 ) ) ;
#3238 = ORIENTED_EDGE ( 'NONE', *, *, #19685, .F. ) ;
#3239 = ORIENTED_EDGE ( 'NONE', *, *, #5107, .T. ) ;
#3240 = ORIENTED_EDGE ( 'NONE', *, *, #13768, .T. ) ;
#3241 = EDGE_CURVE ( 'NONE', #18458, #13936, #4499, .T. ) ;
#3242 = CARTESIAN_POINT ( 'NONE',  ( 0.000000000000000000, 38.00000000000000711, -5.741599279633704455E-16 ) ) ;
#3244 = EDGE_CURVE ( 'NONE', #10515, #9428, #16684, .T. ) ;
#3243 = AXIS2_PLACEMENT_3D ( 'NONE', #4480, #17049, #2908 ) ;
#3245 = ORIENTED_EDGE ( 'NONE', *, *, #10134, .F. ) ;
#3246 = LINE ( 'NONE', #6661, #7711 ) ;
#3247 = ADVANCED_FACE ( 'NONE', ( #20026 ), #1357, .T. ) ;
#3248 = DIRECTION ( 'NONE',  ( 0.000000000000000000, 0.000000000000000000, -1.000000000000000000 ) ) ;
#3249 = DIRECTION ( 'NONE',  ( 1.000000000000000000, 2.135044278125300850E-16, -0.000000000000000000 ) ) ;
#3250 = LINE ( 'NONE', #6457, #13197 ) ;
#3251 = DIRECTION ( 'NONE',  ( 0.000000000000000000, 0.000000000000000000, -1.000000000000000000 ) ) ;
#3252 = SURFACE_STYLE_USAGE ( .BOTH. , #3471 ) ;
#3253 = FILL_AREA_STYLE ('',( #156 ) ) ;
#3254 = VERTEX_POINT ( 'NONE', #15116 ) ;
#3255 = CARTESIAN_POINT ( 'NONE',  ( 0.9999999999999872324, 138.7545334744432637, 488.5655098179835818 ) ) ;
#3256 = FILL_AREA_STYLE_COLOUR ( '', #1317 ) ;
#3257 = DIRECTION ( 'NONE',  ( 1.000000000000000000, 0.000000000000000000, 0.000000000000000000 ) ) ;
#3258 = CARTESIAN_POINT ( 'NONE',  ( 178.4893729001365728, 113.1299228374914918, 170.4174721992565082 ) ) ;
#3259 = DIRECTION ( 'NONE',  ( 0.000000000000000000, 0.000000000000000000, -1.000000000000000000 ) ) ;
#3260 = DIRECTION ( 'NONE',  ( 0.000000000000000000, -1.000000000000000000, 0.000000000000000000 ) ) ;
#3261 =( GEOMETRIC_REPRESENTATION_CONTEXT ( 3 ) GLOBAL_UNCERTAINTY_ASSIGNED_CONTEXT ( ( #17765 ) ) GLOBAL_UNIT_ASSIGNED_CONTEXT ( ( #10329, #15077, #18452 ) ) REPRESENTATION_CONTEXT ( 'NONE', 'WORKASPACE' ) );
#3262 = LINE ( 'NONE', #9644, #9583 ) ;
#3263 = PRESENTATION_LAYER_ASSIGNMENT (  '', '', ( #14125 ) ) ;
#3264 =( NAMED_UNIT ( * ) PLANE_ANGLE_UNIT ( ) SI_UNIT ( $, .RADIAN. ) );
#3265 = ORIENTED_EDGE ( 'NONE', *, *, #9487, .F. ) ;
#3266 = EDGE_CURVE ( 'NONE', #10884, #2779, #962, .T. ) ;
#3267 = ORIENTED_EDGE ( 'NONE', *, *, #5303, .F. ) ;
#3268 = DIRECTION ( 'NONE',  ( -0.000000000000000000, 1.000000000000000000, -0.000000000000000000 ) ) ;
#3269 = CARTESIAN_POINT ( 'NONE',  ( -80.85496986907217831, 140.4048636631002580, 500.8237260975781737 ) ) ;
#3270 = CIRCLE ( 'NONE', #16498, 15.25000000000000000 ) ;
#3271 = VERTEX_POINT ( 'NONE', #6045 ) ;
#3272 = AXIS2_PLACEMENT_3D ( 'NONE', #3912, #12066, #10294 ) ;
#3273 = FILL_AREA_STYLE ('',( #69 ) ) ;
#3274 = COLOUR_RGB ( '', 0.09019608, 0.27058824, 0.51372549) ;
#3275 = CIRCLE ( 'NONE', #13801, 10.00000000000000888 ) ;
#3276 = ORIENTED_EDGE ( 'NONE', *, *, #12264, .F. ) ;
#3277 = CARTESIAN_POINT ( 'NONE',  ( 0.000000000000000000, 306.0487089519832011, -75.00000000000380851 ) ) ;
#3278 = LINE ( 'NONE', #4622, #19800 ) ;
#3279 = CARTESIAN_POINT ( 'NONE',  ( -0.1972064085032595726, 63.00000000000000000, 9.500000000000001776 ) ) ;
#3280 = DIRECTION ( 'NONE',  ( 0.000000000000000000, 0.000000000000000000, -1.000000000000000000 ) ) ;
#3281 = LINE ( 'NONE', #9365, #10308 ) ;
#3282 = CARTESIAN_POINT ( 'NONE',  ( 10.00000000000000000, 301.0487089519826327, 2.148629195649657075E-12 ) ) ;
#3283 = DIRECTION ( 'NONE',  ( 0.000000000000000000, 1.000000000000000000, 0.000000000000000000 ) ) ;
#3284 = DIRECTION ( 'NONE',  ( -1.000000000000000000, 0.000000000000000000, 1.450371633464475582E-15 ) ) ;
#3285 = CARTESIAN_POINT ( 'NONE',  ( 133.4893729001365443, 113.1299228374914634, 220.6387154965113382 ) ) ;
#3286 = PRESENTATION_LAYER_ASSIGNMENT (  '', '', ( #15482 ) ) ;
#3287 = CIRCLE ( 'NONE', #1609, 8.000000000000000000 ) ;
#3288 = COLOUR_RGB ( '', 0.31764706, 0.68627451, 0.89019608) ;
#3289 = EDGE_LOOP ( 'NONE', ( #8007, #17385, #10800, #13124 ) ) ;
#3290 = ORIENTED_EDGE ( 'NONE', *, *, #4726, .F. ) ;
#3291 = SURFACE_STYLE_FILL_AREA ( #15882 ) ;
#3292 = ORIENTED_EDGE ( 'NONE', *, *, #1175, .T. ) ;
#3293 = ORIENTED_EDGE ( 'NONE', *, *, #16438, .T. ) ;
#3294 = ORIENTED_EDGE ( 'NONE', *, *, #18304, .T. ) ;
#3295 = FACE_OUTER_BOUND ( 'NONE', #4028, .T. ) ;
#3296 = CARTESIAN_POINT ( 'NONE',  ( 53.48937290013658696, 123.1299228374914065, 170.4174721992565082 ) ) ;
#3297 = DIRECTION ( 'NONE',  ( 0.000000000000000000, 0.000000000000000000, -1.000000000000000000 ) ) ;
#3298 = CARTESIAN_POINT ( 'NONE',  ( -36.99999999999997868, -20.00000000000000000, -22.99999999999999645 ) ) ;
#3299 = PRESENTATION_LAYER_ASSIGNMENT (  '', '', ( #18422 ) ) ;
#3300 = LINE ( 'NONE', #17409, #5804 ) ;
#3301 = VECTOR ( 'NONE', #8761, 1000.000000000000000 ) ;
#3302 = VERTEX_POINT ( 'NONE', #2931 ) ;
#3303 = DIRECTION ( 'NONE',  ( -1.000000000000000000, 0.000000000000000000, 0.000000000000000000 ) ) ;
#3304 =( NAMED_UNIT ( * ) PLANE_ANGLE_UNIT ( ) SI_UNIT ( $, .RADIAN. ) );
#3305 = DIRECTION ( 'NONE',  ( -0.000000000000000000, -1.000000000000000000, -0.000000000000000000 ) ) ;
#3306 = FILL_AREA_STYLE_COLOUR ( '', #82 ) ;
#3307 = VERTEX_POINT ( 'NONE', #1164 ) ;
#3308 = EDGE_CURVE ( 'NONE', #5827, #2527, #19830, .T. ) ;
#3309 = DIRECTION ( 'NONE',  ( -0.000000000000000000, -1.000000000000000000, -0.000000000000000000 ) ) ;
#3310 = MECHANICAL_DESIGN_GEOMETRIC_PRESENTATION_REPRESENTATION (  '', ( #3659 ), #14829 ) ;
#3311 = AXIS2_PLACEMENT_3D ( 'NONE', #8558, #3928, #19374 ) ;
#3312 = ORIENTED_EDGE ( 'NONE', *, *, #14897, .T. ) ;
#3313 = ADVANCED_FACE ( 'NONE', ( #12213 ), #12120, .T. ) ;
#3314 = DIRECTION ( 'NONE',  ( 0.000000000000000000, -2.352167425053297897E-16, -1.000000000000000000 ) ) ;
#3315 = ORIENTED_EDGE ( 'NONE', *, *, #10147, .F. ) ;
#3316 = FILL_AREA_STYLE_COLOUR ( '', #16299 ) ;
#3317 = PRESENTATION_STYLE_ASSIGNMENT (( #14049 ) ) ;
#3318 = ORIENTED_EDGE ( 'NONE', *, *, #4145, .F. ) ;
#3319 = FACE_OUTER_BOUND ( 'NONE', #178, .T. ) ;
#3320 = SURFACE_STYLE_FILL_AREA ( #18870 ) ;
#3321 = ADVANCED_FACE ( 'NONE', ( #16873 ), #2837, .F. ) ;
#3322 = CIRCLE ( 'NONE', #9248, 3.300000000000011369 ) ;
#3323 = CIRCLE ( 'NONE', #17472, 9.000000000000007105 ) ;
#3324 = CARTESIAN_POINT ( 'NONE',  ( -1.000000012540656069, 140.6662311104242349, 502.2196126213723915 ) ) ;
#3325 = ADVANCED_FACE ( 'NONE', ( #6251, #8105, #17367 ), #6158, .F. ) ;
#3326 = CYLINDRICAL_SURFACE ( 'NONE', #9809, 1.000000000000000888 ) ;
#3327 = PLANE ( 'NONE',  #11346 ) ;
#3328 = DIRECTION ( 'NONE',  ( -5.540106248403443714E-14, 0.06294785234384196737, -0.9980168174361081501 ) ) ;
#3329 = ORIENTED_EDGE ( 'NONE', *, *, #18659, .T. ) ;
#3330 = CARTESIAN_POINT ( 'NONE',  ( 10.00000000000000000, 372.8685141053783241, -146.8198051533979935 ) ) ;
#3331 = DIRECTION ( 'NONE',  ( 1.000000000000000000, -0.000000000000000000, -0.000000000000000000 ) ) ;
#3332 = DIRECTION ( 'NONE',  ( -5.782411586589400040E-16, 0.000000000000000000, 1.000000000000000000 ) ) ;
#3333 = APPLICATION_PROTOCOL_DEFINITION ( 'draft international standard', 'automotive_design', 1998, #1403 ) ;
#3334 = ADVANCED_FACE ( 'NONE', ( #9747 ), #12529, .F. ) ;
#3335 = PRODUCT_DEFINITION_SHAPE ( 'NONE', 'NONE',  #19657 ) ;
#3336 = EDGE_LOOP ( 'NONE', ( #15468, #4072, #768, #5036, #18806, #214 ) ) ;
#3337 = DIRECTION ( 'NONE',  ( -0.000000000000000000, 1.000000000000000000, 0.000000000000000000 ) ) ;
#3338 = EDGE_CURVE ( 'NONE', #2478, #8069, #3353, .T. ) ;
#3339 = ORIENTED_EDGE ( 'NONE', *, *, #12413, .T. ) ;
#3340 = ORIENTED_EDGE ( 'NONE', *, *, #11511, .F. ) ;
#3341 = EDGE_LOOP ( 'NONE', ( #9241, #1562, #8666, #9673 ) ) ;
#3342 = AXIS2_PLACEMENT_3D ( 'NONE', #2307, #17780, #5227 ) ;
#3343 = CARTESIAN_POINT ( 'NONE',  ( 26.00000000000000000, 19.00000000000000000, -40.00000000000000711 ) ) ;
#3344 = EDGE_CURVE ( 'NONE', #8331, #8375, #10879, .T. ) ;
#3345 = COLOUR_RGB ( '', 0.08235294, 0.09019608, 0.10196078) ;
#3346 = ORIENTED_EDGE ( 'NONE', *, *, #16251, .T. ) ;
#3347 = FACE_OUTER_BOUND ( 'NONE', #5595, .T. ) ;
#3348 = CARTESIAN_POINT ( 'NONE',  ( -211.5106270998635409, 103.1299228374912360, 220.6387154965113382 ) ) ;
#3349 = VERTEX_POINT ( 'NONE', #17156 ) ;
#3350 = CARTESIAN_POINT ( 'NONE',  ( 98.48937290013662960, 123.1299228374914350, 79.58252780074349175 ) ) ;
#3351 = PLANE ( 'NONE',  #12256 ) ;
#3352 = DIRECTION ( 'NONE',  ( 1.000000000000000000, 0.000000000000000000, 0.000000000000000000 ) ) ;
#3353 = LINE ( 'NONE', #1478, #3386 ) ;
#3354 = LINE ( 'NONE', #12748, #20244 ) ;
#3355 = EDGE_CURVE ( 'NONE', #8340, #14814, #174, .T. ) ;
#3356 =( NAMED_UNIT ( * ) PLANE_ANGLE_UNIT ( ) SI_UNIT ( $, .RADIAN. ) );
#3357 = CARTESIAN_POINT ( 'NONE',  ( -1.983673311716146026, 38.74097077230339892, 9.291669371308643122 ) ) ;
#3358 = ORIENTED_EDGE ( 'NONE', *, *, #17075, .T. ) ;
#3359 = DIRECTION ( 'NONE',  ( -0.000000000000000000, 1.000000000000000000, -0.000000000000000000 ) ) ;
#3360 = DIRECTION ( 'NONE',  ( -1.000000000000000000, -0.000000000000000000, -0.000000000000000000 ) ) ;
#3361 = DIRECTION ( 'NONE',  ( 0.000000000000000000, -1.000000000000000000, 0.000000000000000000 ) ) ;
#3362 = CIRCLE ( 'NONE', #8313, 0.6999999999999992895 ) ;
#3363 = FACE_OUTER_BOUND ( 'NONE', #7853, .T. ) ;
#3364 = CARTESIAN_POINT ( 'NONE',  ( -81.00000000000260059, 139.7703989349477354, 490.5655098180907885 ) ) ;
#3365 = ADVANCED_FACE ( 'NONE', ( #12634 ), #18502, .T. ) ;
#3366 = CARTESIAN_POINT ( 'NONE',  ( -79.99999999999995737, 216.7545334744432921, 478.3411705753777596 ) ) ;
#3367 = CARTESIAN_POINT ( 'NONE',  ( -0.2803133411605864267, 138.8192838135785507, 489.9877526172908233 ) ) ;
#3368 = EDGE_LOOP ( 'NONE', ( #952, #2526, #18692, #3681, #11719 ) ) ;
#3369 = VECTOR ( 'NONE', #11615, 1000.000000000000000 ) ;
#3370 = ORIENTED_EDGE ( 'NONE', *, *, #6922, .F. ) ;
#3371 = SURFACE_STYLE_USAGE ( .BOTH. , #4518 ) ;
#3372 = AXIS2_PLACEMENT_3D ( 'NONE', #6696, #1915, #13102 ) ;
#3373 = CARTESIAN_POINT ( 'NONE',  ( -78.99999999591139499, 140.6663224100674370, 502.2197208097303474 ) ) ;
#3374 = CIRCLE ( 'NONE', #14891, 10.00000000000000888 ) ;
#3375 = ORIENTED_EDGE ( 'NONE', *, *, #7006, .T. ) ;
#3376 = DIRECTION ( 'NONE',  ( 0.000000000000000000, -0.000000000000000000, 1.000000000000000000 ) ) ;
#3377 = CARTESIAN_POINT ( 'NONE',  ( 53.48937290013658696, 122.8810204491430369, 280.0825295754780768 ) ) ;
#3378 = VECTOR ( 'NONE', #18387, 1000.000000000000000 ) ;
#3379 = ADVANCED_FACE ( 'NONE', ( #7886 ), #6016, .T. ) ;
#3380 = ORIENTED_EDGE ( 'NONE', *, *, #1445, .F. ) ;
#3381 = LINE ( 'NONE', #6803, #17772 ) ;
#3382 = CARTESIAN_POINT ( 'NONE',  ( 10.00000000000000000, 372.8685141053778693, -83.18019484660869978 ) ) ;
#3383 = CARTESIAN_POINT ( 'NONE',  ( 53.48937290013659407, 211.0574367717017594, 346.4752554294135507 ) ) ;
#3384 = CARTESIAN_POINT ( 'NONE',  ( -20.99999999999999645, 19.00000000000000000, 35.00000000000001421 ) ) ;
#3385 = LINE ( 'NONE', #9973, #14942 ) ;
#3386 = VECTOR ( 'NONE', #4595, 1000.000000000000000 ) ;
#3387 = MECHANICAL_DESIGN_GEOMETRIC_PRESENTATION_REPRESENTATION (  '', ( #8647 ), #1372 ) ;
#3388 = CARTESIAN_POINT ( 'NONE',  ( 30.99999999999995737, 0.000000000000000000, 31.00000000000000000 ) ) ;
#3389 = DIRECTION ( 'NONE',  ( 0.000000000000000000, 0.000000000000000000, 1.000000000000000000 ) ) ;
#3390 = DIRECTION ( 'NONE',  ( 0.000000000000000000, -1.000000000000000000, 0.000000000000000000 ) ) ;
#3391 = DIRECTION ( 'NONE',  ( -1.000000000000000000, -0.000000000000000000, -0.000000000000000000 ) ) ;
#3392 = CARTESIAN_POINT ( 'NONE',  ( -37.00000000000000711, 10.00000000000000000, 23.00000000000000000 ) ) ;
#3393 = LINE ( 'NONE', #2969, #15790 ) ;
#3394 = ORIENTED_EDGE ( 'NONE', *, *, #3207, .F. ) ;
#3395 = AXIS2_PLACEMENT_3D ( 'NONE', #8837, #13575, #17072 ) ;
#3396 = MECHANICAL_DESIGN_GEOMETRIC_PRESENTATION_REPRESENTATION (  '', ( #9634 ), #14865 ) ;
#3397 = ORIENTED_EDGE ( 'NONE', *, *, #5756, .T. ) ;
#3398 =( BOUNDED_SURFACE ( )  B_SPLINE_SURFACE ( 3, 2, ( 
 ( #17897, #18192, #16387 ),
 ( #10269, #8619, #16686 ),
 ( #6805, #2536, #11517 ),
 ( #9971, #2221, #16476 ),
 ( #15022, #778, #18090 ),
 ( #19340, #3798, #2129 ),
 ( #19725, #10168, #7102 ),
 ( #16285, #679, #17797 ),
 ( #3987, #4098, #3689 ),
 ( #8441, #2432, #8738 ),
 ( #2325, #14717, #6899 ),
 ( #587, #875, #5537 ) ),
 .UNSPECIFIED., .F., .F., .T. ) 
 B_SPLINE_SURFACE_WITH_KNOTS ( ( 4, 2, 2, 2, 2, 4 ),
 ( 3, 3 ),
 ( 0.001513949667275679917, 0.002304520018506476739, 0.002699805194121875258, 0.003095090369737273344, 0.003885660720968069949, 0.004676231072198866988 ),
 ( 0.000000000000000000, 1.000000000000000000 ),
 .UNSPECIFIED. ) 
 GEOMETRIC_REPRESENTATION_ITEM ( )  RATIONAL_B_SPLINE_SURFACE ( (
 ( 1.000000000000000000, 0.7071067811865475727, 1.000000000000000000),
 ( 1.000000000000000000, 0.7210992828362334794, 1.000000000000000000),
 ( 1.000000000000000000, 0.7304325578646034822, 1.000000000000000000),
 ( 1.000000000000000000, 0.7381509264279376703, 1.000000000000000000),
 ( 1.000000000000000000, 0.7396729138149117366, 1.000000000000000000),
 ( 1.000000000000000000, 0.7411282974412637392, 1.000000000000000000),
 ( 1.000000000000000000, 0.7410425863960605763, 1.000000000000000000),
 ( 1.000000000000000000, 0.7392589090250264450, 1.000000000000000000),
 ( 1.000000000000000000, 0.7360636976591894420, 1.000000000000000000),
 ( 1.000000000000000000, 0.7309106356142509586, 1.000000000000000000),
 ( 1.000000000000000000, 0.7289402462822450746, 1.000000000000000000),
 ( 1.000000000000000000, 0.7290225827585891105, 1.000000000000000000) ) ) 
 REPRESENTATION_ITEM ( '' )  SURFACE ( )  );
#3399 = EDGE_LOOP ( 'NONE', ( #2269, #19922, #1471, #12921 ) ) ;
#3400 = UNCERTAINTY_MEASURE_WITH_UNIT (LENGTH_MEASURE( 1.000000000000000082E-05 ), #11505, 'distance_accuracy_value', 'NONE');
#3401 = CLOSED_SHELL ( 'NONE', ( #19100, #18033, #138, #2470, #8067, #14919, #10517, #4991, #4858, #11404, #4207, #3325, #2584, #8762, #14077, #8973, #9314, #18177, #14932, #11058, #11196, #12679, #15273, #10854, #9492, #9665, #20058, #7880, #1638, #47, #1316, #2772, #19974, #3825, #4224, #17857, #7509, #17172, #7025, #14765, #15164, #4717, #18684, #16776, #4577, #17293, #10804, #4250, #12276, #17873, #3365, #6522, #2476, #6348, #12630, #12232, #4848, #8479, #4406, #10661, #12525, #19827, #20209, #12640, #11242, #15428, #17807, #17729, #12972, #2274, #4053, #14542 ) ) ;
#3402 = EDGE_LOOP ( 'NONE', ( #7232, #2254 ) ) ;
#3403 =( GEOMETRIC_REPRESENTATION_CONTEXT ( 3 ) GLOBAL_UNCERTAINTY_ASSIGNED_CONTEXT ( ( #7010 ) ) GLOBAL_UNIT_ASSIGNED_CONTEXT ( ( #11834, #8336, #15027 ) ) REPRESENTATION_CONTEXT ( 'NONE', 'WORKASPACE' ) );
#3404 = ORIENTED_EDGE ( 'NONE', *, *, #8914, .F. ) ;
#3405 = CARTESIAN_POINT ( 'NONE',  ( 0.000000000000000000, 50.00000000000000000, 0.000000000000000000 ) ) ;
#3406 = FILL_AREA_STYLE ('',( #17500 ) ) ;
#3407 = VECTOR ( 'NONE', #12755, 1000.000000000000000 ) ;
#3408 = CARTESIAN_POINT ( 'NONE',  ( 25.99999999999996092, 3.000000000000000000, -33.99999999999998579 ) ) ;
#3409 = DIRECTION ( 'NONE',  ( 1.000000000000000000, 0.000000000000000000, 0.000000000000000000 ) ) ;
#3410 = ORIENTED_EDGE ( 'NONE', *, *, #9631, .T. ) ;
#3411 = PRESENTATION_STYLE_ASSIGNMENT (( #1937 ) ) ;
#3412 = CARTESIAN_POINT ( 'NONE',  ( 22.99999999999995737, 3.000000000000000000, -33.99999999999998579 ) ) ;
#3413 = FILL_AREA_STYLE_COLOUR ( '', #2709 ) ;
#3414 = PRESENTATION_STYLE_ASSIGNMENT (( #6512 ) ) ;
#3415 = EDGE_CURVE ( 'NONE', #758, #12917, #9630, .T. ) ;
#3416 =( GEOMETRIC_REPRESENTATION_CONTEXT ( 3 ) GLOBAL_UNCERTAINTY_ASSIGNED_CONTEXT ( ( #2509 ) ) GLOBAL_UNIT_ASSIGNED_CONTEXT ( ( #4318, #12244, #1283 ) ) REPRESENTATION_CONTEXT ( 'NONE', 'WORKASPACE' ) );
#3417 = EDGE_LOOP ( 'NONE', ( #7184, #8490, #3882, #2569 ) ) ;
#3418 = VECTOR ( 'NONE', #12248, 1000.000000000000000 ) ;
#3419 = FACE_OUTER_BOUND ( 'NONE', #16911, .T. ) ;
#3420 = LINE ( 'NONE', #6730, #19548 ) ;
#3421 = VECTOR ( 'NONE', #779, 1000.000000000000000 ) ;
#3422 = ORIENTED_EDGE ( 'NONE', *, *, #8631, .F. ) ;
#3423 = PRESENTATION_STYLE_ASSIGNMENT (( #19286 ) ) ;
#3424 = ORIENTED_EDGE ( 'NONE', *, *, #2722, .T. ) ;
#3425 = STYLED_ITEM ( 'NONE', ( #5194 ), #1489 ) ;
#3426 = SURFACE_STYLE_USAGE ( .BOTH. , #6428 ) ;
#3427 = MECHANICAL_DESIGN_GEOMETRIC_PRESENTATION_REPRESENTATION (  '', ( #4095 ), #11320 ) ;
#3428 = ORIENTED_EDGE ( 'NONE', *, *, #14826, .F. ) ;
#3429 = EDGE_CURVE ( 'NONE', #9184, #4662, #5009, .T. ) ;
#3430 = FACE_OUTER_BOUND ( 'NONE', #19624, .T. ) ;
#3431 = ORIENTED_EDGE ( 'NONE', *, *, #19425, .F. ) ;
#3432 = VECTOR ( 'NONE', #11482, 1000.000000000000000 ) ;
#3433 = CYLINDRICAL_SURFACE ( 'NONE', #16012, 3.000000000000009770 ) ;
#3434 = FILL_AREA_STYLE_COLOUR ( '', #734 ) ;
#3435 = AXIS2_PLACEMENT_3D ( 'NONE', #6540, #17438, #3332 ) ;
#3436 = MECHANICAL_DESIGN_GEOMETRIC_PRESENTATION_REPRESENTATION (  '', ( #2113 ), #19874 ) ;
#3437 = CARTESIAN_POINT ( 'NONE',  ( 0.08008856490587368260, 141.0493802267578474, 501.4268783641182381 ) ) ;
#3438 = DIRECTION ( 'NONE',  ( -0.000000000000000000, -1.000000000000000000, -0.000000000000000000 ) ) ;
#3439 = DIRECTION ( 'NONE',  ( 0.000000000000000000, 0.000000000000000000, -1.000000000000000000 ) ) ;
#3440 = DIRECTION ( 'NONE',  ( 1.000000000000000000, -0.000000000000000000, -0.000000000000000000 ) ) ;
#3441 = VERTEX_POINT ( 'NONE', #12747 ) ;
#3442 = CARTESIAN_POINT ( 'NONE',  ( 10.00000000000000000, 309.2289037985885898, -86.48019484660916589 ) ) ;
#3443 = DIRECTION ( 'NONE',  ( 0.000000000000000000, 0.000000000000000000, 1.000000000000000000 ) ) ;
#3444 = DIRECTION ( 'NONE',  ( 1.000000000000000000, -0.000000000000000000, 0.000000000000000000 ) ) ;
#3445 = EDGE_CURVE ( 'NONE', #5831, #10467, #4902, .T. ) ;
#3446 = EDGE_LOOP ( 'NONE', ( #20105, #7303, #18238, #2213, #14566, #19545 ) ) ;
#3447 = PRESENTATION_LAYER_ASSIGNMENT (  '', '', ( #12323 ) ) ;
#3448 = FACE_OUTER_BOUND ( 'NONE', #14593, .T. ) ;
#3449 = ORIENTED_EDGE ( 'NONE', *, *, #2580, .F. ) ;
#3450 = AXIS2_PLACEMENT_3D ( 'NONE', #6219, #12715, #3220 ) ;
#3451 = EDGE_LOOP ( 'NONE', ( #12616, #12969, #12450 ) ) ;
#3452 = EDGE_CURVE ( 'NONE', #15858, #6545, #8789, .T. ) ;
#3453 = ORIENTED_EDGE ( 'NONE', *, *, #1295, .F. ) ;
#3454 = CIRCLE ( 'NONE', #14975, 2.500000000000002220 ) ;
#3455 = VECTOR ( 'NONE', #16116, 1000.000000000000000 ) ;
#3456 = ORIENTED_EDGE ( 'NONE', *, *, #12594, .F. ) ;
#3457 =( GEOMETRIC_REPRESENTATION_CONTEXT ( 3 ) GLOBAL_UNCERTAINTY_ASSIGNED_CONTEXT ( ( #416 ) ) GLOBAL_UNIT_ASSIGNED_CONTEXT ( ( #13486, #11931, #8839 ) ) REPRESENTATION_CONTEXT ( 'NONE', 'WORKASPACE' ) );
#3458 = CIRCLE ( 'NONE', #14980, 1.000000000000000888 ) ;
#3459 = FACE_OUTER_BOUND ( 'NONE', #16103, .T. ) ;
#3460 = EDGE_LOOP ( 'NONE', ( #12134, #15489, #13261, #3083, #19207 ) ) ;
#3461 = CARTESIAN_POINT ( 'NONE',  ( -44.50085094405407915, 159.0821755739672483, 505.3921618609452935 ) ) ;
#3462 = LINE ( 'NONE', #19311, #7553 ) ;
#3463 = VERTEX_POINT ( 'NONE', #13525 ) ;
#3464 = EDGE_CURVE ( 'NONE', #8069, #19923, #14692, .T. ) ;
#3465 = DIRECTION ( 'NONE',  ( -1.000000000000000000, 0.000000000000000000, 0.000000000000000000 ) ) ;
#3466 = PRESENTATION_LAYER_ASSIGNMENT (  '', '', ( #10054 ) ) ;
#3467 = EDGE_CURVE ( 'NONE', #9680, #13739, #7338, .T. ) ;
#3468 = CARTESIAN_POINT ( 'NONE',  ( 53.48937290013659407, 145.9162550801369491, 250.0000000000000000 ) ) ;
#3469 = CIRCLE ( 'NONE', #5123, 0.9999999999999974465 ) ;
#3470 = DIRECTION ( 'NONE',  ( 1.000000000000000000, 5.889072920838430686E-16, -0.000000000000000000 ) ) ;
#3471 = SURFACE_SIDE_STYLE ('',( #7991 ) ) ;
#3472 = CARTESIAN_POINT ( 'NONE',  ( 108.9893729001366296, 130.3113892758443910, 284.0770112900635240 ) ) ;
#3473 = CARTESIAN_POINT ( 'NONE',  ( -2.259918635623970218, 39.01734001413205277, 9.228371864727252571 ) ) ;
#3474 = ORIENTED_EDGE ( 'NONE', *, *, #18592, .T. ) ;
#3475 = CARTESIAN_POINT ( 'NONE',  ( 0.000000000000000000, 301.0487089519832011, -80.00000000000387956 ) ) ;
#3476 = FILL_AREA_STYLE_COLOUR ( '', #12893 ) ;
#3477 = CARTESIAN_POINT ( 'NONE',  ( -44.50085094405407915, 175.4489062796178871, 505.3921618609452935 ) ) ;
#3478 = MECHANICAL_DESIGN_GEOMETRIC_PRESENTATION_REPRESENTATION (  '', ( #823 ), #13665 ) ;
#3479 = ADVANCED_FACE ( 'NONE', ( #7153 ), #5581, .T. ) ;
#3480 =( LENGTH_UNIT ( ) NAMED_UNIT ( * ) SI_UNIT ( .MILLI., .METRE. ) );
#3481 = VERTEX_POINT ( 'NONE', #838 ) ;
#3482 = VERTEX_POINT ( 'NONE', #3566 ) ;
#3483 = VECTOR ( 'NONE', #2623, 1000.000000000000000 ) ;
#3484 = EDGE_CURVE ( 'NONE', #14793, #18509, #20148, .T. ) ;
#3485 = EDGE_LOOP ( 'NONE', ( #1245, #14570 ) ) ;
#3486 = FILL_AREA_STYLE ('',( #479 ) ) ;
#3487 = CARTESIAN_POINT ( 'NONE',  ( 0.000000000000000000, -3.000000000000000888, -150.0000000000000000 ) ) ;
#3488 = ORIENTED_EDGE ( 'NONE', *, *, #502, .F. ) ;
#3489 = EDGE_CURVE ( 'NONE', #17522, #16867, #14578, .T. ) ;
#3490 = FACE_OUTER_BOUND ( 'NONE', #2308, .T. ) ;
#3491 = DIRECTION ( 'NONE',  ( 1.000000000000000000, 0.000000000000000000, 0.000000000000000000 ) ) ;
#3492 = ADVANCED_FACE ( 'NONE', ( #18250 ), #4249, .F. ) ;
#3493 = ORIENTED_EDGE ( 'NONE', *, *, #20034, .T. ) ;
#3494 = LINE ( 'NONE', #11305, #6269 ) ;
#3495 = CARTESIAN_POINT ( 'NONE',  ( 1.469576158976824144E-15, 10.00000000000000000, 12.00000000000000178 ) ) ;
#3496 = VECTOR ( 'NONE', #9893, 1000.000000000000000 ) ;
#3497 =( LENGTH_UNIT ( ) NAMED_UNIT ( * ) SI_UNIT ( .MILLI., .METRE. ) );
#3498 = FACE_BOUND ( 'NONE', #13047, .T. ) ;
#3499 = VECTOR ( 'NONE', #9793, 1000.000000000000000 ) ;
#3500 = DIRECTION ( 'NONE',  ( 0.000000000000000000, 0.000000000000000000, 1.000000000000000000 ) ) ;
#3501 = DIRECTION ( 'NONE',  ( 1.000000000000000000, 0.000000000000000000, -0.000000000000000000 ) ) ;
#3502 = CARTESIAN_POINT ( 'NONE',  ( 26.00000000000000711, 68.00000000000000000, -31.00000000000002487 ) ) ;
#3503 = DIRECTION ( 'NONE',  ( 1.000000000000000000, 0.000000000000000000, 0.000000000000000000 ) ) ;
#3504 = CARTESIAN_POINT ( 'NONE',  ( 53.48937290013659407, 145.9162550801369491, 250.0000000000000000 ) ) ;
#3505 = ORIENTED_EDGE ( 'NONE', *, *, #16960, .T. ) ;
#3506 = VERTEX_POINT ( 'NONE', #9091 ) ;
#3507 = VERTEX_POINT ( 'NONE', #1530 ) ;
#3508 =( GEOMETRIC_REPRESENTATION_CONTEXT ( 3 ) GLOBAL_UNCERTAINTY_ASSIGNED_CONTEXT ( ( #14660 ) ) GLOBAL_UNIT_ASSIGNED_CONTEXT ( ( #19557, #16609, #3913 ) ) REPRESENTATION_CONTEXT ( 'NONE', 'WORKASPACE' ) );
#3509 = CARTESIAN_POINT ( 'NONE',  ( 40.00000000000001421, 0.000000000000000000, -150.0000000000000000 ) ) ;
#3510 = EDGE_LOOP ( 'NONE', ( #6417, #9656, #7137, #11391, #18853 ) ) ;
#3511 = ADVANCED_FACE ( 'NONE', ( #18658 ), #18849, .F. ) ;
#3512 = ORIENTED_EDGE ( 'NONE', *, *, #3680, .F. ) ;
#3513 = CARTESIAN_POINT ( 'NONE',  ( 178.4893729001365443, 145.9162550801369491, 250.0000000000000000 ) ) ;
#3514 = AXIS2_PLACEMENT_3D ( 'NONE', #7305, #2148, #14731 ) ;
#3515 = PRESENTATION_STYLE_ASSIGNMENT (( #204 ) ) ;
#3516 = LINE ( 'NONE', #18843, #19199 ) ;
#3517 = SURFACE_STYLE_FILL_AREA ( #9795 ) ;
#3518 = EDGE_CURVE ( 'NONE', #19410, #7140, #10293, .T. ) ;
#3519 = DIRECTION ( 'NONE',  ( -0.000000000000000000, -0.000000000000000000, 1.000000000000000000 ) ) ;
#3520 = CARTESIAN_POINT ( 'NONE',  ( 149.0892156028631348, 80.91625508013694912, 250.0000000000000000 ) ) ;
#3521 = CARTESIAN_POINT ( 'NONE',  ( 0.7824566857511728868, 62.90282673968097527, 9.469691317190790159 ) ) ;
#3522 =( LENGTH_UNIT ( ) NAMED_UNIT ( * ) SI_UNIT ( .MILLI., .METRE. ) );
#3523 = PLANE ( 'NONE',  #8060 ) ;
#3524 = FILL_AREA_STYLE ('',( #2039 ) ) ;
#3525 = FACE_OUTER_BOUND ( 'NONE', #7407, .T. ) ;
#3526 = DIRECTION ( 'NONE',  ( 0.000000000000000000, 0.7642367632649269549, -0.6449357872488920007 ) ) ;
#3527 = DIRECTION ( 'NONE',  ( 0.000000000000000000, 0.000000000000000000, -1.000000000000000000 ) ) ;
#3528 = CIRCLE ( 'NONE', #14050, 1.000000000000015987 ) ;
#3529 = ORIENTED_EDGE ( 'NONE', *, *, #5590, .T. ) ;
#3530 = LINE ( 'NONE', #19172, #15659 ) ;
#3531 = ORIENTED_EDGE ( 'NONE', *, *, #4472, .F. ) ;
#3532 = EDGE_CURVE ( 'NONE', #11785, #17808, #4448, .T. ) ;
#3533 = LINE ( 'NONE', #14441, #7284 ) ;
#3534 = ORIENTED_EDGE ( 'NONE', *, *, #49, .T. ) ;
#3535 = CARTESIAN_POINT ( 'NONE',  ( 133.4893729001365443, 103.1299228374914492, 29.36128450348865471 ) ) ;
#3536 = CARTESIAN_POINT ( 'NONE',  ( -79.99999999999995737, 152.4824555358011082, 478.3411705753777596 ) ) ;
#3537 = UNCERTAINTY_MEASURE_WITH_UNIT (LENGTH_MEASURE( 1.000000000000000082E-05 ), #6314, 'distance_accuracy_value', 'NONE');
#3538 = ORIENTED_EDGE ( 'NONE', *, *, #8692, .F. ) ;
#3539 = DIRECTION ( 'NONE',  ( -0.000000000000000000, -0.000000000000000000, 1.000000000000000000 ) ) ;
#3540 = SURFACE_STYLE_USAGE ( .BOTH. , #17653 ) ;
#3541 = DIRECTION ( 'NONE',  ( -1.000000000000000000, 0.000000000000000000, 1.017652531801993019E-13 ) ) ;
#3542 = DIRECTION ( 'NONE',  ( 0.000000000000000000, 0.000000000000000000, 1.000000000000000000 ) ) ;
#3543 = DIRECTION ( 'NONE',  ( 1.000000000000000000, 0.000000000000000000, 0.000000000000000000 ) ) ;
#3544 = ORIENTED_EDGE ( 'NONE', *, *, #11891, .F. ) ;
#3545 = FACE_OUTER_BOUND ( 'NONE', #19371, .T. ) ;
#3546 = CARTESIAN_POINT ( 'NONE',  ( 0.000000000000000000, 138.7545334744432637, 491.0690926367356042 ) ) ;
#3547 = CARTESIAN_POINT ( 'NONE',  ( 22.99999999999999289, 68.00000000000000000, 37.00000000000002132 ) ) ;
#3548 = ITEM_DEFINED_TRANSFORMATION ( 'NONE', 'NONE', #8363,  #2741 ) ;
#3549 = ORIENTED_EDGE ( 'NONE', *, *, #2189, .T. ) ;
#3550 = CIRCLE ( 'NONE', #241, 18.50000000000000000 ) ;
#3551 = CARTESIAN_POINT ( 'NONE',  ( -82.18192946989277914, 138.7545334744432637, 500.8237260975782874 ) ) ;
#3552 = APPLICATION_CONTEXT ( 'automotive_design' ) ;
#3553 = ORIENTED_EDGE ( 'NONE', *, *, #20294, .F. ) ;
#3554 = ORIENTED_EDGE ( 'NONE', *, *, #17144, .T. ) ;
#3555 = ORIENTED_EDGE ( 'NONE', *, *, #3464, .T. ) ;
#3556 = CARTESIAN_POINT ( 'NONE',  ( 498.8117674897343932, 191.8198460455371333, 81.76606011801540319 ) ) ;
#3557 = DIRECTION ( 'NONE',  ( 1.000000000000000000, 0.000000000000000000, 0.000000000000000000 ) ) ;
#3558 = ORIENTED_EDGE ( 'NONE', *, *, #18842, .F. ) ;
#3559 = CIRCLE ( 'NONE', #19647, 4.999999999999997335 ) ;
#3560 = SURFACE_STYLE_FILL_AREA ( #2191 ) ;
#3561 = CARTESIAN_POINT ( 'NONE',  ( 0.4745977552357285023, 139.7919181881820236, 489.4271902104604237 ) ) ;
#3562 = ORIENTED_EDGE ( 'NONE', *, *, #13673, .F. ) ;
#3563 = EDGE_CURVE ( 'NONE', #11798, #7874, #7542, .T. ) ;
#3564 = LINE ( 'NONE', #8204, #2721 ) ;
#3565 = VECTOR ( 'NONE', #6283, 1000.000000000000000 ) ;
#3566 = CARTESIAN_POINT ( 'NONE',  ( -35.00000000000000000, 8.000000000000000000, 20.99999999999999289 ) ) ;
#3567 = DIRECTION ( 'NONE',  ( 0.000000000000000000, 0.000000000000000000, -1.000000000000000000 ) ) ;
#3568 = CARTESIAN_POINT ( 'NONE',  ( 0.000000000000000000, 50.00000000000000000, 0.000000000000000000 ) ) ;
#3569 = PRODUCT_RELATED_PRODUCT_CATEGORY ( 'part', '', ( #7941 ) ) ;
#3570 = ORIENTED_EDGE ( 'NONE', *, *, #1513, .F. ) ;
#3571 = DIRECTION ( 'NONE',  ( -0.000000000000000000, -1.000000000000000000, -0.000000000000000000 ) ) ;
#3572 = CARTESIAN_POINT ( 'NONE',  ( 22.99999999999998224, 0.000000000000000000, -31.00000000000003197 ) ) ;
#3573 = LINE ( 'NONE', #661, #7682 ) ;
#3574 = DIRECTION ( 'NONE',  ( 1.000000000000000000, 0.000000000000000000, 0.000000000000000000 ) ) ;
#3575 = LINE ( 'NONE', #8317, #6977 ) ;
#3576 = DIRECTION ( 'NONE',  ( 0.000000000000000000, 0.000000000000000000, -1.000000000000000000 ) ) ;
#3577 = EDGE_CURVE ( 'NONE', #13735, #16276, #6207, .T. ) ;
#3578 = ORIENTED_EDGE ( 'NONE', *, *, #9762, .T. ) ;
#3579 = CIRCLE ( 'NONE', #17719, 10.00000000000001066 ) ;
#3580 = ORIENTED_EDGE ( 'NONE', *, *, #3671, .F. ) ;
#3581 = VERTEX_POINT ( 'NONE', #13921 ) ;
#3582 = DIRECTION ( 'NONE',  ( 1.000000000000000000, -0.000000000000000000, -0.000000000000000000 ) ) ;
#3583 = CARTESIAN_POINT ( 'NONE',  ( -80.81398221677214622, 139.7462607834860648, 500.8237260972081799 ) ) ;
#3584 = ORIENTED_EDGE ( 'NONE', *, *, #18299, .T. ) ;
#3585 = ADVANCED_FACE ( 'NONE', ( #12481 ), #9393, .F. ) ;
#3586 = DIRECTION ( 'NONE',  ( 0.000000000000000000, 1.000000000000000000, 0.000000000000000000 ) ) ;
#3587 = EDGE_CURVE ( 'NONE', #1243, #63, #4343, .T. ) ;
#3588 = DIRECTION ( 'NONE',  ( 0.000000000000000000, -1.000000000000000000, 0.000000000000000000 ) ) ;
#3589 = VERTEX_POINT ( 'NONE', #15593 ) ;
#3590 = CARTESIAN_POINT ( 'NONE',  ( 35.99999999999999289, 8.000000000000000000, 18.99999999999999289 ) ) ;
#3591 = CARTESIAN_POINT ( 'NONE',  ( -23.00000000000002132, 10.00000000000000000, 37.00000000000000711 ) ) ;
#3592 = PRESENTATION_STYLE_ASSIGNMENT (( #17297 ) ) ;
#3593 = MECHANICAL_DESIGN_GEOMETRIC_PRESENTATION_REPRESENTATION (  '', ( #20352 ), #17732 ) ;
#3594 = DIRECTION ( 'NONE',  ( 1.000000000000000000, -0.000000000000000000, -0.000000000000000000 ) ) ;
#3595 = EDGE_CURVE ( 'NONE', #16084, #4680, #1370, .T. ) ;
#3596 = DIRECTION ( 'NONE',  ( 1.450371633464475582E-15, 0.000000000000000000, 1.000000000000000000 ) ) ;
#3597 = SHAPE_REPRESENTATION_RELATIONSHIP ( 'NONE' , 'NONE' ,  #8923, #524 ) ;
#3598 = SURFACE_SIDE_STYLE ('',( #13189 ) ) ;
#3599 = EDGE_CURVE ( 'NONE', #1878, #792, #9302, .T. ) ;
#3600 = PLANE ( 'NONE',  #14223 ) ;
#3601 = CYLINDRICAL_SURFACE ( 'NONE', #15451, 4.999999999999997335 ) ;
#3602 = LINE ( 'NONE', #14723, #10234 ) ;
#3603 = CYLINDRICAL_SURFACE ( 'NONE', #19705, 10.00000000000000888 ) ;
#3604 = ORIENTED_EDGE ( 'NONE', *, *, #2318, .T. ) ;
#3605 = EDGE_CURVE ( 'NONE', #18105, #20055, #15702, .T. ) ;
#3606 = VERTEX_POINT ( 'NONE', #15381 ) ;
#3607 = MECHANICAL_DESIGN_GEOMETRIC_PRESENTATION_REPRESENTATION (  '', ( #5612 ), #7581 ) ;
#3608 = ORIENTED_EDGE ( 'NONE', *, *, #19563, .F. ) ;
#3609 = STYLED_ITEM ( 'NONE', ( #18162 ), #11043 ) ;
#3610 = VERTEX_POINT ( 'NONE', #12172 ) ;
#3611 = VERTEX_POINT ( 'NONE', #15272 ) ;
#3612 = CARTESIAN_POINT ( 'NONE',  ( -34.99999999999999289, 0.000000000000000000, 35.00000000000000711 ) ) ;
#3613 = EDGE_CURVE ( 'NONE', #6600, #4111, #18549, .T. ) ;
#3614 = CARTESIAN_POINT ( 'NONE',  ( 498.8334540492693918, 214.2156642432025251, 250.0000000000000000 ) ) ;
#3615 = DIRECTION ( 'NONE',  ( 0.000000000000000000, -1.000000000000000000, 0.000000000000000000 ) ) ;
#3616 = DIRECTION ( 'NONE',  ( 1.000000000000000000, 0.000000000000000000, 0.000000000000000000 ) ) ;
#3617 = PLANE ( 'NONE',  #4728 ) ;
#3618 = LINE ( 'NONE', #19280, #7825 ) ;
#3619 =( GEOMETRIC_REPRESENTATION_CONTEXT ( 3 ) GLOBAL_UNCERTAINTY_ASSIGNED_CONTEXT ( ( #6837 ) ) GLOBAL_UNIT_ASSIGNED_CONTEXT ( ( #2473, #19761, #18229 ) ) REPRESENTATION_CONTEXT ( 'NONE', 'WORKASPACE' ) );
#3620 = SURFACE_SIDE_STYLE ('',( #13015 ) ) ;
#3621 = DIRECTION ( 'NONE',  ( 1.000000000000000000, 9.815121534730717399E-17, -0.000000000000000000 ) ) ;
#3622 = FILL_AREA_STYLE ('',( #11450 ) ) ;
#3623 = CIRCLE ( 'NONE', #5272, 9.500000000000000000 ) ;
#3624 = CARTESIAN_POINT ( 'NONE',  ( 5.162501635565829972, 0.000000000000000000, 0.000000000000000000 ) ) ;
#3625 = EDGE_CURVE ( 'NONE', #9522, #3885, #13820, .T. ) ;
#3626 = CYLINDRICAL_SURFACE ( 'NONE', #20207, 9.500000000000000000 ) ;
#3627 = EDGE_CURVE ( 'NONE', #16599, #1681, #17215, .T. ) ;
#3628 = VERTEX_POINT ( 'NONE', #15485 ) ;
#3629 =( NAMED_UNIT ( * ) PLANE_ANGLE_UNIT ( ) SI_UNIT ( $, .RADIAN. ) );
#3630 = ORIENTED_EDGE ( 'NONE', *, *, #6654, .F. ) ;
#3631 = STYLED_ITEM ( 'NONE', ( #18404 ), #16376 ) ;
#3632 = VECTOR ( 'NONE', #13182, 1000.000000000000000 ) ;
#3633 = AXIS2_PLACEMENT_3D ( 'NONE', #322, #17946, #16422 ) ;
#3634 = FILL_AREA_STYLE_COLOUR ( '', #6300 ) ;
#3635 = EDGE_LOOP ( 'NONE', ( #15087, #9200, #2212, #9055 ) ) ;
#3636 = CARTESIAN_POINT ( 'NONE',  ( -1.387778780781445676E-14, 138.7545334744432637, 489.5655098179848892 ) ) ;
#3637 = DIRECTION ( 'NONE',  ( 0.000000000000000000, 0.7071067811865336949, -0.7071067811865614505 ) ) ;
#3638 = VERTEX_POINT ( 'NONE', #2790 ) ;
#3639 = DIRECTION ( 'NONE',  ( 1.000000000000000000, 0.000000000000000000, 0.000000000000000000 ) ) ;
#3640 = CARTESIAN_POINT ( 'NONE',  ( 178.4893729001365728, 113.1299228374914918, 220.6387154965113382 ) ) ;
#3641 = SURFACE_SIDE_STYLE ('',( #3849 ) ) ;
#3642 =( NAMED_UNIT ( * ) SI_UNIT ( $, .STERADIAN. ) SOLID_ANGLE_UNIT ( ) );
#3643 = FACE_OUTER_BOUND ( 'NONE', #6297, .T. ) ;
#3644 = VERTEX_POINT ( 'NONE', #17027 ) ;
#3645 =( NAMED_UNIT ( * ) SI_UNIT ( $, .STERADIAN. ) SOLID_ANGLE_UNIT ( ) );
#3646 = DIRECTION ( 'NONE',  ( -0.000000000000000000, -0.000000000000000000, -1.000000000000000000 ) ) ;
#3647 = LINE ( 'NONE', #3547, #1759 ) ;
#3648 = VECTOR ( 'NONE', #10811, 1000.000000000000000 ) ;
#3649 = AXIS2_PLACEMENT_3D ( 'NONE', #7984, #2656, #12744 ) ;
#3650 = VECTOR ( 'NONE', #1962, 1000.000000000000000 ) ;
#3651 = AXIS2_PLACEMENT_3D ( 'NONE', #14115, #1, #14427 ) ;
#3652 = CARTESIAN_POINT ( 'NONE',  ( 503.8334540492693918, 242.8734308960556234, 0.000000000000000000 ) ) ;
#3653 = EDGE_LOOP ( 'NONE', ( #16572, #10093, #1441, #12892 ) ) ;
#3654 = VECTOR ( 'NONE', #12249, 1000.000000000000000 ) ;
#3655 = EDGE_LOOP ( 'NONE', ( #6547, #16380, #11267, #4807 ) ) ;
#3656 = ORIENTED_EDGE ( 'NONE', *, *, #18201, .T. ) ;
#3657 = LINE ( 'NONE', #12079, #16330 ) ;
#3658 = ORIENTED_EDGE ( 'NONE', *, *, #19355, .F. ) ;
#3659 = STYLED_ITEM ( 'NONE', ( #6139 ), #16856 ) ;
#3660 = DIRECTION ( 'NONE',  ( -0.000000000000000000, -1.000000000000000000, -0.000000000000000000 ) ) ;
#3661 = ORIENTED_EDGE ( 'NONE', *, *, #923, .F. ) ;
#3662 = VECTOR ( 'NONE', #3314, 1000.000000000000000 ) ;
#3663 = DIRECTION ( 'NONE',  ( -1.000000000000000000, -9.815121534730717399E-17, 0.000000000000000000 ) ) ;
#3664 = PRESENTATION_STYLE_ASSIGNMENT (( #5417 ) ) ;
#3665 = SURFACE_STYLE_USAGE ( .BOTH. , #9845 ) ;
#3666 = CARTESIAN_POINT ( 'NONE',  ( -1.334572366541263433, 38.30595095619238322, 9.407584458684455697 ) ) ;
#3667 = ORIENTED_EDGE ( 'NONE', *, *, #1737, .F. ) ;
#3668 = DIRECTION ( 'NONE',  ( 6.123031769111888756E-17, 0.000000000000000000, 1.000000000000000000 ) ) ;
#3669 = DIRECTION ( 'NONE',  ( 1.000000000000000000, 0.000000000000000000, -0.000000000000000000 ) ) ;
#3670 =( NAMED_UNIT ( * ) SI_UNIT ( $, .STERADIAN. ) SOLID_ANGLE_UNIT ( ) );
#3671 = EDGE_CURVE ( 'NONE', #12734, #6007, #4650, .T. ) ;
#3672 = VERTEX_POINT ( 'NONE', #12389 ) ;
#3673 = CARTESIAN_POINT ( 'NONE',  ( 0.000000000000000000, 341.0487089519837696, -96.50000000000331113 ) ) ;
#3674 = EDGE_LOOP ( 'NONE', ( #6199, #8988, #15111, #19349, #5136, #18507, #19814, #6846 ) ) ;
#3675 = VECTOR ( 'NONE', #13616, 1000.000000000000000 ) ;
#3676 = EDGE_LOOP ( 'NONE', ( #19396, #18917, #10092, #1296 ) ) ;
#3677 = VERTEX_POINT ( 'NONE', #1426 ) ;
#3678 = CARTESIAN_POINT ( 'NONE',  ( 30.99999999999999645, 0.000000000000000000, 31.00000000000001066 ) ) ;
#3679 = CARTESIAN_POINT ( 'NONE',  ( 0.000000000000000000, 309.2289037985885898, -83.18019484660915452 ) ) ;
#3680 = EDGE_CURVE ( 'NONE', #10206, #9680, #7638, .T. ) ;
#3681 = ORIENTED_EDGE ( 'NONE', *, *, #317, .T. ) ;
#3682 = CARTESIAN_POINT ( 'NONE',  ( 1.181929469893326257, 138.7545334744432637, 500.8237260975781737 ) ) ;
#3683 = SURFACE_STYLE_FILL_AREA ( #2123 ) ;
#3684 = EDGE_LOOP ( 'NONE', ( #14648, #7737 ) ) ;
#3685 = EDGE_CURVE ( 'NONE', #4282, #664, #14034, .T. ) ;
#3686 = DIRECTION ( 'NONE',  ( 0.000000000000000000, 0.000000000000000000, 1.000000000000000000 ) ) ;
#3687 = VECTOR ( 'NONE', #10155, 1000.000000000000000 ) ;
#3688 = CARTESIAN_POINT ( 'NONE',  ( -3.000000000000000000, -1.836909530733565148E-16, 3.000000000000000000 ) ) ;
#3689 = CARTESIAN_POINT ( 'NONE',  ( -0.01728972014804384949, 138.7946624528599671, 490.2123583867289653 ) ) ;
#3690 = SURFACE_STYLE_USAGE ( .BOTH. , #13098 ) ;
#3691 = AXIS2_PLACEMENT_3D ( 'NONE', #3678, #8323, #17788 ) ;
#3692 = CARTESIAN_POINT ( 'NONE',  ( -211.5106270998635409, 123.1299228374912644, 170.4174721992565082 ) ) ;
#3693 =( NAMED_UNIT ( * ) PLANE_ANGLE_UNIT ( ) SI_UNIT ( $, .RADIAN. ) );
#3694 = PLANE ( 'NONE',  #5111 ) ;
#3695 = LINE ( 'NONE', #14812, #1022 ) ;
#3696 = DIRECTION ( 'NONE',  ( 0.000000000000000000, 0.000000000000000000, -1.000000000000000000 ) ) ;
#3697 =( LENGTH_UNIT ( ) NAMED_UNIT ( * ) SI_UNIT ( .MILLI., .METRE. ) );
#3698 = ORIENTED_EDGE ( 'NONE', *, *, #9646, .F. ) ;
#3699 = ADVANCED_FACE ( 'NONE', ( #19361 ), #1873, .T. ) ;
#3700 = AXIS2_PLACEMENT_3D ( 'NONE', #18733, #4629, #17193 ) ;
#3701 = PRESENTATION_LAYER_ASSIGNMENT (  '', '', ( #5017 ) ) ;
#3702 = PRODUCT_DEFINITION_CONTEXT ( 'detailed design', #3552, 'design' ) ;
#3703 = ORIENTED_EDGE ( 'NONE', *, *, #7005, .T. ) ;
#3704 = ADVANCED_FACE ( 'NONE', ( #14337 ), #2034, .F. ) ;
#3705 = MECHANICAL_DESIGN_GEOMETRIC_PRESENTATION_REPRESENTATION (  '', ( #12239 ), #15219 ) ;
#3706 = ORIENTED_EDGE ( 'NONE', *, *, #16349, .F. ) ;
#3707 = ORIENTED_EDGE ( 'NONE', *, *, #7763, .F. ) ;
#3708 = LINE ( 'NONE', #5652, #2510 ) ;
#3709 = FACE_OUTER_BOUND ( 'NONE', #3336, .T. ) ;
#3710 = LINE ( 'NONE', #7120, #112 ) ;
#3711 = AXIS2_PLACEMENT_3D ( 'NONE', #3382, #18820, #17389 ) ;
#3712 = AXIS2_PLACEMENT_3D ( 'NONE', #1740, #3305, #12585 ) ;
#3713 = CARTESIAN_POINT ( 'NONE',  ( 78.48937290013660117, 123.1299228374914208, 29.36128450348865471 ) ) ;
#3714 = EDGE_CURVE ( 'NONE', #4513, #6680, #3550, .T. ) ;
#3715 = CARTESIAN_POINT ( 'NONE',  ( -44.50085094405409336, 193.0431417881923153, 505.3921618609452935 ) ) ;
#3716 = DIRECTION ( 'NONE',  ( -0.000000000000000000, -1.000000000000000000, -0.000000000000000000 ) ) ;
#3717 = CARTESIAN_POINT ( 'NONE',  ( 78.48937290013660117, 103.1299228374914065, 170.4174721992565082 ) ) ;
#3718 = EDGE_CURVE ( 'NONE', #7492, #7254, #9577, .T. ) ;
#3719 = AXIS2_PLACEMENT_3D ( 'NONE', #12537, #12338, #7592 ) ;
#3720 = STYLED_ITEM ( 'NONE', ( #5016 ), #18322 ) ;
#3721 = DIRECTION ( 'NONE',  ( 6.123031769111888756E-17, 0.000000000000000000, 1.000000000000000000 ) ) ;
#3722 = DIRECTION ( 'NONE',  ( -0.000000000000000000, 0.7071067811865455743, 0.7071067811865493491 ) ) ;
#3723 = CIRCLE ( 'NONE', #17860, 8.000000000000000000 ) ;
#3724 = SURFACE_SIDE_STYLE ('',( #8548 ) ) ;
#3725 = CARTESIAN_POINT ( 'NONE',  ( -1.135258727068402232E-15, 138.7545334744432637, 478.3411705753777596 ) ) ;
#3726 = EDGE_CURVE ( 'NONE', #19976, #2341, #9450, .T. ) ;
#3727 = AXIS2_PLACEMENT_3D ( 'NONE', #16925, #8975, #2989 ) ;
#3728 = ORIENTED_EDGE ( 'NONE', *, *, #9001, .F. ) ;
#3729 = UNCERTAINTY_MEASURE_WITH_UNIT (LENGTH_MEASURE( 1.000000000000000082E-05 ), #17342, 'distance_accuracy_value', 'NONE');
#3730 = ORIENTED_EDGE ( 'NONE', *, *, #2571, .T. ) ;
#3731 = PRESENTATION_LAYER_ASSIGNMENT (  '', '', ( #16889 ) ) ;
#3732 = EDGE_CURVE ( 'NONE', #4111, #4175, #401, .T. ) ;
#3733 = ORIENTED_EDGE ( 'NONE', *, *, #173, .T. ) ;
#3734 = LINE ( 'NONE', #6840, #16497 ) ;
#3735 = ORIENTED_EDGE ( 'NONE', *, *, #6001, .F. ) ;
#3736 = UNCERTAINTY_MEASURE_WITH_UNIT (LENGTH_MEASURE( 1.000000000000000082E-05 ), #8161, 'distance_accuracy_value', 'NONE');
#3737 = CARTESIAN_POINT ( 'NONE',  ( 0.000000000000000000, 0.000000000000000000, 0.000000000000000000 ) ) ;
#3738 = LINE ( 'NONE', #10120, #11197 ) ;
#3739 = ORIENTED_EDGE ( 'NONE', *, *, #12267, .F. ) ;
#3740 = EDGE_CURVE ( 'NONE', #6449, #5650, #18961, .T. ) ;
#3741 = DIRECTION ( 'NONE',  ( -0.000000000000000000, -1.000000000000000000, -0.000000000000000000 ) ) ;
#3742 = VECTOR ( 'NONE', #16904, 1000.000000000000000 ) ;
#3743 =( LENGTH_UNIT ( ) NAMED_UNIT ( * ) SI_UNIT ( .MILLI., .METRE. ) );
#3744 = LINE ( 'NONE', #13043, #16563 ) ;
#3745 = FILL_AREA_STYLE ('',( #633 ) ) ;
#3746 = ORIENTED_EDGE ( 'NONE', *, *, #903, .T. ) ;
#3747 = DIRECTION ( 'NONE',  ( 0.000000000000000000, 0.000000000000000000, -1.000000000000000000 ) ) ;
#3748 = AXIS2_PLACEMENT_3D ( 'NONE', #6925, #3716, #9999 ) ;
#3749 = VECTOR ( 'NONE', #10153, 1000.000000000000000 ) ;
#3750 = EDGE_LOOP ( 'NONE', ( #17447, #18910, #9268, #18739 ) ) ;
#3751 = AXIS2_PLACEMENT_3D ( 'NONE', #8705, #2513, #19606 ) ;
#3752 = PRESENTATION_LAYER_ASSIGNMENT (  '', '', ( #9643 ) ) ;
#3753 = EDGE_CURVE ( 'NONE', #11075, #13854, #12433, .T. ) ;
#3754 = EDGE_LOOP ( 'NONE', ( #10562, #15236, #6709, #12889 ) ) ;
#3755 = ORIENTED_EDGE ( 'NONE', *, *, #435, .T. ) ;
#3756 = VECTOR ( 'NONE', #7577, 1000.000000000000000 ) ;
#3757 = FACE_OUTER_BOUND ( 'NONE', #13643, .T. ) ;
#3758 = EDGE_LOOP ( 'NONE', ( #7656, #578, #19030, #526, #4213, #15922 ) ) ;
#3759 = UNCERTAINTY_MEASURE_WITH_UNIT (LENGTH_MEASURE( 1.000000000000000082E-05 ), #7160, 'distance_accuracy_value', 'NONE');
#3760 = ADVANCED_FACE ( 'NONE', ( #102 ), #12798, .F. ) ;
#3761 = CIRCLE ( 'NONE', #7054, 0.9999999999999950040 ) ;
#3762 =( LENGTH_UNIT ( ) NAMED_UNIT ( * ) SI_UNIT ( .MILLI., .METRE. ) );
#3763 = PRESENTATION_LAYER_ASSIGNMENT (  '', '', ( #18871 ) ) ;
#3764 = CARTESIAN_POINT ( 'NONE',  ( 0.9714722756524812874, 38.15493332361022283, 9.451944983354378493 ) ) ;
#3765 = VECTOR ( 'NONE', #2686, 1000.000000000000000 ) ;
#3766 = ORIENTED_EDGE ( 'NONE', *, *, #17198, .F. ) ;
#3767 = DIRECTION ( 'NONE',  ( 0.000000000000000000, 0.000000000000000000, -1.000000000000000000 ) ) ;
#3768 = AXIS2_PLACEMENT_3D ( 'NONE', #16742, #2592, #18557 ) ;
#3769 = CARTESIAN_POINT ( 'NONE',  ( 0.000000000000000000, 316.7545334744432353, 515.1946179577817020 ) ) ;
#3770 = LINE ( 'NONE', #10148, #1244 ) ;
#3771 = SPHERICAL_SURFACE ( 'NONE', #10026, 1.000000000000000000 ) ;
#3772 = AXIS2_PLACEMENT_3D ( 'NONE', #17318, #10936, #4854 ) ;
#3773 = EDGE_LOOP ( 'NONE', ( #12751, #2703, #7272, #19122, #17170 ) ) ;
#3774 = PRESENTATION_STYLE_ASSIGNMENT (( #11593 ) ) ;
#3775 = AXIS2_PLACEMENT_3D ( 'NONE', #7519, #7719, #7819 ) ;
#3776 = DIRECTION ( 'NONE',  ( 0.000000000000000000, 0.000000000000000000, -1.000000000000000000 ) ) ;
#3777 = PRESENTATION_LAYER_ASSIGNMENT (  '', '', ( #16304 ) ) ;
#3778 = ORIENTED_EDGE ( 'NONE', *, *, #4971, .F. ) ;
#3779 = AXIS2_PLACEMENT_3D ( 'NONE', #17330, #17223, #9490 ) ;
#3780 = CIRCLE ( 'NONE', #472, 10.00000000000000888 ) ;
#3781 = EDGE_CURVE ( 'NONE', #10287, #688, #17505, .T. ) ;
#3782 = ORIENTED_EDGE ( 'NONE', *, *, #7636, .T. ) ;
#3783 = ORIENTED_EDGE ( 'NONE', *, *, #1418, .T. ) ;
#3784 = CIRCLE ( 'NONE', #18563, 2.000000000000001776 ) ;
#3785 = MECHANICAL_DESIGN_GEOMETRIC_PRESENTATION_REPRESENTATION (  '', ( #12323 ), #2784 ) ;
#3786 = ORIENTED_EDGE ( 'NONE', *, *, #689, .T. ) ;
#3787 = DIRECTION ( 'NONE',  ( 0.000000000000000000, 0.000000000000000000, -1.000000000000000000 ) ) ;
#3788 = CARTESIAN_POINT ( 'NONE',  ( 40.00000000000000000, 0.000000000000000000, 26.00000000000000355 ) ) ;
#3789 = ORIENTED_EDGE ( 'NONE', *, *, #15038, .T. ) ;
#3790 = CARTESIAN_POINT ( 'NONE',  ( 36.99999999999999289, 10.00000000000000000, 22.99999999999999645 ) ) ;
#3791 = ADVANCED_FACE ( 'NONE', ( #12905 ), #17725, .F. ) ;
#3792 = DIRECTION ( 'NONE',  ( 7.714700791774674864E-14, 0.000000000000000000, 1.000000000000000000 ) ) ;
#3793 = EDGE_LOOP ( 'NONE', ( #5869, #12117, #19031, #12665 ) ) ;
#3794 = STYLED_ITEM ( 'NONE', ( #9415 ), #12872 ) ;
#3795 = CARTESIAN_POINT ( 'NONE',  ( -64.99999999999995737, 316.7545334744432353, 475.1454018718993098 ) ) ;
#3796 = COLOUR_RGB ( '', 0.72549020, 0.75294118, 0.79215686) ;
#3797 = DIRECTION ( 'NONE',  ( -0.000000000000000000, -1.000000000000000000, -0.000000000000000000 ) ) ;
#3798 = CARTESIAN_POINT ( 'NONE',  ( 0.1267668549151080015, 138.9617779728525875, 489.0733406692675089 ) ) ;
#3799 = CIRCLE ( 'NONE', #11365, 10.00000000000000888 ) ;
#3800 = DIRECTION ( 'NONE',  ( -1.000000000000000000, 0.000000000000000000, 0.000000000000000000 ) ) ;
#3801 = CARTESIAN_POINT ( 'NONE',  ( 10.00000000000000000, 309.2289037985885898, -83.18019484660915452 ) ) ;
#3802 =( LENGTH_UNIT ( ) NAMED_UNIT ( * ) SI_UNIT ( .MILLI., .METRE. ) );
#3803 = CARTESIAN_POINT ( 'NONE',  ( 22.99999999999995737, 3.000000000000000000, -33.99999999999998579 ) ) ;
#3804 = AXIS2_PLACEMENT_3D ( 'NONE', #7230, #19575, #13608 ) ;
#3805 = CARTESIAN_POINT ( 'NONE',  ( -3.000000000000002220, 60.00000000000000711, 6.000000000000000000 ) ) ;
#3806 = ORIENTED_EDGE ( 'NONE', *, *, #16140, .T. ) ;
#3807 = DIRECTION ( 'NONE',  ( 0.000000000000000000, 0.000000000000000000, 1.000000000000000000 ) ) ;
#3808 = CARTESIAN_POINT ( 'NONE',  ( 21.99999999999998224, 10.00000000000000000, -31.99999999999998579 ) ) ;
#3809 = ORIENTED_EDGE ( 'NONE', *, *, #5580, .F. ) ;
#3810 = ORIENTED_EDGE ( 'NONE', *, *, #14053, .T. ) ;
#3811 = EDGE_CURVE ( 'NONE', #14904, #15622, #3618, .T. ) ;
#3812 = ORIENTED_EDGE ( 'NONE', *, *, #5148, .T. ) ;
#3813 = VECTOR ( 'NONE', #15167, 1000.000000000000000 ) ;
#3814 = ORIENTED_EDGE ( 'NONE', *, *, #15974, .T. ) ;
#3815 = ORIENTED_EDGE ( 'NONE', *, *, #7279, .T. ) ;
#3816 =( LENGTH_UNIT ( ) NAMED_UNIT ( * ) SI_UNIT ( .MILLI., .METRE. ) );
#3817 = VECTOR ( 'NONE', #5681, 1000.000000000000000 ) ;
#3818 = DIRECTION ( 'NONE',  ( 0.000000000000000000, 1.000000000000000000, 0.000000000000000000 ) ) ;
#3819 = CARTESIAN_POINT ( 'NONE',  ( 0.000000000000000000, -5.000000000000000888, 0.000000000000000000 ) ) ;
#3820 = CARTESIAN_POINT ( 'NONE',  ( -78.99999999999995737, 138.7545334744432637, 478.3411705753777596 ) ) ;
#3821 = PRESENTATION_STYLE_ASSIGNMENT (( #5556 ) ) ;
#3822 = MECHANICAL_DESIGN_GEOMETRIC_PRESENTATION_REPRESENTATION (  '', ( #1139 ), #5810 ) ;
#3823 = CARTESIAN_POINT ( 'NONE',  ( -79.99999999999995737, 216.7545334744432921, 477.3411705753777596 ) ) ;
#3825 = ADVANCED_FACE ( 'NONE', ( #5176 ), #11447, .T. ) ;
#3824 = LINE ( 'NONE', #14336, #7037 ) ;
#3826 = DIRECTION ( 'NONE',  ( 0.000000000000000000, -0.000000000000000000, 1.000000000000000000 ) ) ;
#3827 = CARTESIAN_POINT ( 'NONE',  ( -32.00000000000000711, 10.00000000000000000, -22.00000000000000355 ) ) ;
#3828 = FACE_OUTER_BOUND ( 'NONE', #17980, .T. ) ;
#3829 = PLANE ( 'NONE',  #7397 ) ;
#3830 =( GEOMETRIC_REPRESENTATION_CONTEXT ( 3 ) GLOBAL_UNCERTAINTY_ASSIGNED_CONTEXT ( ( #11360 ) ) GLOBAL_UNIT_ASSIGNED_CONTEXT ( ( #17025, #1306, #20194 ) ) REPRESENTATION_CONTEXT ( 'NONE', 'WORKASPACE' ) );
#3831 = EDGE_CURVE ( 'NONE', #8449, #19193, #11545, .T. ) ;
#3832 = ORIENTED_EDGE ( 'NONE', *, *, #3563, .T. ) ;
#3833 = CIRCLE ( 'NONE', #20275, 10.00000000000000888 ) ;
#3834 = ORIENTED_EDGE ( 'NONE', *, *, #11303, .F. ) ;
#3835 = CARTESIAN_POINT ( 'NONE',  ( -44.50085094405409336, 193.0431417881923153, 510.3921618609452935 ) ) ;
#3836 = VERTEX_POINT ( 'NONE', #2559 ) ;
#3837 = VERTEX_POINT ( 'NONE', #7021 ) ;
#3838 = EDGE_CURVE ( 'NONE', #18751, #9451, #6926, .T. ) ;
#3839 = VECTOR ( 'NONE', #13791, 1000.000000000000227 ) ;
#3840 = ORIENTED_EDGE ( 'NONE', *, *, #8136, .T. ) ;
#3841 = CARTESIAN_POINT ( 'NONE',  ( -79.99999999999995737, 216.7545334744432921, 495.1946179577816451 ) ) ;
#3842 = ORIENTED_EDGE ( 'NONE', *, *, #9922, .T. ) ;
#3843 = LINE ( 'NONE', #16424, #17000 ) ;
#3844 = CARTESIAN_POINT ( 'NONE',  ( 31.00000000000004263, 68.00000000000000000, -25.99999999999999645 ) ) ;
#3846 = ADVANCED_FACE ( 'NONE', ( #13597 ), #16315, .T. ) ;
#3845 = CARTESIAN_POINT ( 'NONE',  ( -81.18192946989263703, 138.7545334744432637, 496.6642397995874489 ) ) ;
#3847 = VECTOR ( 'NONE', #8612, 1000.000000000000000 ) ;
#3848 = LINE ( 'NONE', #11780, #9075 ) ;
#3849 = SURFACE_STYLE_FILL_AREA ( #14668 ) ;
#3850 = DIRECTION ( 'NONE',  ( -0.000000000000000000, -0.000000000000000000, 1.000000000000000000 ) ) ;
#3851 = CARTESIAN_POINT ( 'NONE',  ( 26.00000000000000000, 11.00000000000000000, 31.00000000000003197 ) ) ;
#3852 = EDGE_CURVE ( 'NONE', #2362, #12596, #5659, .T. ) ;
#3853 = ORIENTED_EDGE ( 'NONE', *, *, #17964, .F. ) ;
#3854 = PLANE ( 'NONE',  #16117 ) ;
#3855 = CARTESIAN_POINT ( 'NONE',  ( 10.00000000000000000, 309.2289037985890445, -146.8198051533984199 ) ) ;
#3856 = DIRECTION ( 'NONE',  ( 5.782411586589399054E-16, 0.000000000000000000, -1.000000000000000000 ) ) ;
#3857 = EDGE_CURVE ( 'NONE', #11725, #2115, #18022, .T. ) ;
#3858 = EDGE_CURVE ( 'NONE', #9680, #13902, #17691, .T. ) ;
#3859 = ORIENTED_EDGE ( 'NONE', *, *, #847, .F. ) ;
#3860 = EDGE_LOOP ( 'NONE', ( #15760, #15520, #4413, #16399, #14899, #12203 ) ) ;
#3861 = ORIENTED_EDGE ( 'NONE', *, *, #16026, .F. ) ;
#3862 =( NAMED_UNIT ( * ) PLANE_ANGLE_UNIT ( ) SI_UNIT ( $, .RADIAN. ) );
#3863 = CYLINDRICAL_SURFACE ( 'NONE', #14149, 3.299999999999997158 ) ;
#3864 = ORIENTED_EDGE ( 'NONE', *, *, #13419, .F. ) ;
#3865 = DIRECTION ( 'NONE',  ( 1.000000000000000000, 0.000000000000000000, -0.000000000000000000 ) ) ;
#3866 =( LENGTH_UNIT ( ) NAMED_UNIT ( * ) SI_UNIT ( .MILLI., .METRE. ) );
#3867 = PRESENTATION_STYLE_ASSIGNMENT (( #352 ) ) ;
#3868 = UNCERTAINTY_MEASURE_WITH_UNIT (LENGTH_MEASURE( 1.000000000000000082E-05 ), #2343, 'distance_accuracy_value', 'NONE');
#3869 = CYLINDRICAL_SURFACE ( 'NONE', #17935, 10.00000000000000888 ) ;
#3870 = CARTESIAN_POINT ( 'NONE',  ( -38.50085094405407204, 175.4489062796178871, 510.3921618609452935 ) ) ;
#3871 = CARTESIAN_POINT ( 'NONE',  ( 133.4893729001365443, 113.1299228374914634, 220.6387154965113382 ) ) ;
#3872 = COLOUR_RGB ( '', 0.72549020, 0.75294118, 0.79215686) ;
#3873 = VERTEX_POINT ( 'NONE', #14740 ) ;
#3874 = CYLINDRICAL_SURFACE ( 'NONE', #5229, 1.000000000000000888 ) ;
#3875 = PLANE ( 'NONE',  #11938 ) ;
#3876 = CARTESIAN_POINT ( 'NONE',  ( -37.00000000000000711, 10.00000000000000000, 23.00000000000000000 ) ) ;
#3877 = SHAPE_REPRESENTATION_RELATIONSHIP ( 'NONE' , 'NONE' ,  #13798, #13320 ) ;
#3878 = LINE ( 'NONE', #11498, #9937 ) ;
#3879 = EDGE_CURVE ( 'NONE', #4081, #10815, #11856, .T. ) ;
#3880 = ORIENTED_EDGE ( 'NONE', *, *, #7969, .F. ) ;
#3881 = EDGE_CURVE ( 'NONE', #12403, #5525, #16730, .T. ) ;
#3882 = ORIENTED_EDGE ( 'NONE', *, *, #4995, .T. ) ;
#3883 = ADVANCED_FACE ( 'NONE', ( #11648 ), #17927, .F. ) ;
#3884 = CIRCLE ( 'NONE', #18995, 2.000000000000001776 ) ;
#3885 = VERTEX_POINT ( 'NONE', #2355 ) ;
#3886 = VERTEX_POINT ( 'NONE', #8766 ) ;
#3887 = DIRECTION ( 'NONE',  ( -0.000000000000000000, -1.000000000000000000, 0.000000000000000000 ) ) ;
#3888 = CARTESIAN_POINT ( 'NONE',  ( -1.000000000000012657, 140.1563709946295262, 488.5655098179835818 ) ) ;
#3889 = ORIENTED_EDGE ( 'NONE', *, *, #13535, .T. ) ;
#3890 = DIRECTION ( 'NONE',  ( -1.000000000000000000, 0.000000000000000000, 0.000000000000000000 ) ) ;
#3891 = PRESENTATION_STYLE_ASSIGNMENT (( #17996 ) ) ;
#3892 =( LENGTH_UNIT ( ) NAMED_UNIT ( * ) SI_UNIT ( .MILLI., .METRE. ) );
#3893 = DIRECTION ( 'NONE',  ( -1.000000000000000000, 0.000000000000000000, -0.000000000000000000 ) ) ;
#3894 =( LENGTH_UNIT ( ) NAMED_UNIT ( * ) SI_UNIT ( .MILLI., .METRE. ) );
#3895 =( NAMED_UNIT ( * ) PLANE_ANGLE_UNIT ( ) SI_UNIT ( $, .RADIAN. ) );
#3896 = FACE_OUTER_BOUND ( 'NONE', #2374, .T. ) ;
#3897 = DIRECTION ( 'NONE',  ( 0.000000000000000000, 0.000000000000000000, -1.000000000000000000 ) ) ;
#3898 = FACE_OUTER_BOUND ( 'NONE', #4437, .T. ) ;
#3899 = DIRECTION ( 'NONE',  ( 0.000000000000000000, 0.000000000000000000, -1.000000000000000000 ) ) ;
#3900 = CIRCLE ( 'NONE', #5873, 10.00000000000000888 ) ;
#3901 =( NAMED_UNIT ( * ) SI_UNIT ( $, .STERADIAN. ) SOLID_ANGLE_UNIT ( ) );
#3902 = ORIENTED_EDGE ( 'NONE', *, *, #17916, .T. ) ;
#3903 = EDGE_CURVE ( 'NONE', #11436, #9454, #813, .T. ) ;
#3904 = VERTEX_POINT ( 'NONE', #5470 ) ;
#3905 = PRODUCT_DEFINITION_CONTEXT ( 'detailed design', #2871, 'design' ) ;
#3906 = ORIENTED_EDGE ( 'NONE', *, *, #10622, .F. ) ;
#3907 = ORIENTED_EDGE ( 'NONE', *, *, #5767, .F. ) ;
#3908 = VERTEX_POINT ( 'NONE', #2243 ) ;
#3909 = PLANE ( 'NONE',  #16297 ) ;
#3910 = DIRECTION ( 'NONE',  ( -0.000000000000000000, -1.000000000000000000, -0.000000000000000000 ) ) ;
#3911 = DIRECTION ( 'NONE',  ( -0.000000000000000000, 0.000000000000000000, -1.000000000000000000 ) ) ;
#3912 = CARTESIAN_POINT ( 'NONE',  ( 2.999999999999996891, 60.00000000000000711, 6.000000000000000000 ) ) ;
#3913 =( NAMED_UNIT ( * ) SI_UNIT ( $, .STERADIAN. ) SOLID_ANGLE_UNIT ( ) );
#3914 = CARTESIAN_POINT ( 'NONE',  ( 503.8334540492693918, 191.8198460455371333, 225.0057801310552463 ) ) ;
#3915 = CARTESIAN_POINT ( 'NONE',  ( 423.8334540492694487, 191.8198460455371333, 14.99421986894475012 ) ) ;
#3916 = DIRECTION ( 'NONE',  ( -0.000000000000000000, -1.000000000000000000, -0.000000000000000000 ) ) ;
#3917 = FACE_OUTER_BOUND ( 'NONE', #17261, .T. ) ;
#3918 = AXIS2_PLACEMENT_3D ( 'NONE', #2797, #9097, #16190 ) ;
#3919 =( GEOMETRIC_REPRESENTATION_CONTEXT ( 3 ) GLOBAL_UNCERTAINTY_ASSIGNED_CONTEXT ( ( #12686 ) ) GLOBAL_UNIT_ASSIGNED_CONTEXT ( ( #16546, #16161, #1988 ) ) REPRESENTATION_CONTEXT ( 'NONE', 'WORKASPACE' ) );
#3920 = ORIENTED_EDGE ( 'NONE', *, *, #18599, .T. ) ;
#3921 = EDGE_LOOP ( 'NONE', ( #7354, #4003, #11072, #8822 ) ) ;
#3922 = SURFACE_STYLE_USAGE ( .BOTH. , #11767 ) ;
#3923 = UNCERTAINTY_MEASURE_WITH_UNIT (LENGTH_MEASURE( 1.000000000000000082E-05 ), #15280, 'distance_accuracy_value', 'NONE');
#3924 = EDGE_LOOP ( 'NONE', ( #9913, #2396, #1039, #16592 ) ) ;
#3925 = EDGE_LOOP ( 'NONE', ( #3081, #8088, #11459, #5820 ) ) ;
#3926 = VERTEX_POINT ( 'NONE', #3717 ) ;
#3927 = DIRECTION ( 'NONE',  ( 1.000000000000000000, 5.889072920838430686E-16, -0.000000000000000000 ) ) ;
#3928 = DIRECTION ( 'NONE',  ( 0.000000000000000000, 1.000000000000000000, 0.000000000000000000 ) ) ;
#3929 = UNCERTAINTY_MEASURE_WITH_UNIT (LENGTH_MEASURE( 1.000000000000000082E-05 ), #10782, 'distance_accuracy_value', 'NONE');
#3930 = APPLICATION_CONTEXT ( 'automotive_design' ) ;
#3931 = FILL_AREA_STYLE ('',( #15065 ) ) ;
#3932 = CIRCLE ( 'NONE', #12493, 10.00000000000000888 ) ;
#3933 = EDGE_LOOP ( 'NONE', ( #11920, #16508, #1142, #18920, #7489, #16854, #3340, #2421, #13698, #6768, #5791, #1045, #7979, #2218, #8813, #13971, #4715, #18740, #3422, #19594, #4823, #1820, #1754, #7058 ) ) ;
#3934 = SHAPE_REPRESENTATION ( 'Part10^Assem2', ( #2741 ), #5722 ) ;
#3935 = PLANE ( 'NONE',  #523 ) ;
#3936 = STYLED_ITEM ( 'NONE', ( #3821 ), #6510 ) ;
#3937 = CIRCLE ( 'NONE', #13168, 4.999999999999997335 ) ;
#3938 = ADVANCED_FACE ( 'NONE', ( #8542 ), #11759, .F. ) ;
#3939 = CARTESIAN_POINT ( 'NONE',  ( 17.99999999999998224, 10.00000000000000000, -35.99999999999999289 ) ) ;
#3940 = CARTESIAN_POINT ( 'NONE',  ( 2.181929469893224560, 138.7545334744432637, 499.8237260975781169 ) ) ;
#3941 = CARTESIAN_POINT ( 'NONE',  ( -25.99999999999999645, 0.000000000000000000, -39.99999999999999289 ) ) ;
#3942 = ORIENTED_EDGE ( 'NONE', *, *, #12512, .T. ) ;
#3943 = DIRECTION ( 'NONE',  ( 0.000000000000000000, 0.000000000000000000, 1.000000000000000000 ) ) ;
#3944 = SURFACE_SIDE_STYLE ('',( #14868 ) ) ;
#3945 = DIRECTION ( 'NONE',  ( 0.000000000000000000, -0.000000000000000000, 1.000000000000000000 ) ) ;
#3946 = VECTOR ( 'NONE', #11293, 1000.000000000000000 ) ;
#3947 = AXIS2_PLACEMENT_3D ( 'NONE', #6586, #14302, #1908 ) ;
#3948 = EDGE_CURVE ( 'NONE', #11627, #7970, #703, .T. ) ;
#3949 = CIRCLE ( 'NONE', #15484, 3.299999999999997158 ) ;
#3950 = ORIENTED_EDGE ( 'NONE', *, *, #11254, .T. ) ;
#3951 = EDGE_LOOP ( 'NONE', ( #1413, #4610 ) ) ;
#3952 = EDGE_CURVE ( 'NONE', #593, #9818, #5559, .T. ) ;
#3953 = ORIENTED_EDGE ( 'NONE', *, *, #18444, .F. ) ;
#3954 = CARTESIAN_POINT ( 'NONE',  ( 108.9893729001366154, 95.58236431990637527, 327.6194023386000822 ) ) ;
#3955 = DIRECTION ( 'NONE',  ( 1.000000000000000000, 0.000000000000000000, -7.709882115452498874E-16 ) ) ;
#3956 = ORIENTED_EDGE ( 'NONE', *, *, #7600, .F. ) ;
#3957 = EDGE_CURVE ( 'NONE', #10947, #243, #15047, .T. ) ;
#3958 = CARTESIAN_POINT ( 'NONE',  ( 0.000000000000000000, 66.00000000000000000, 0.000000000000000000 ) ) ;
#3959 = CARTESIAN_POINT ( 'NONE',  ( -80.99999999999995737, 139.4861549369088323, 500.2186618848270996 ) ) ;
#3960 = SURFACE_STYLE_USAGE ( .BOTH. , #15090 ) ;
#3961 = COLOUR_RGB ( '', 0.08235294, 0.09019608, 0.10196078) ;
#3962 = CARTESIAN_POINT ( 'NONE',  ( -58.16843972078500258, 317.7545334744432353, 485.1700099148404206 ) ) ;
#3963 = AXIS2_PLACEMENT_3D ( 'NONE', #2150, #14939, #16404 ) ;
#3964 = DIRECTION ( 'NONE',  ( 0.000000000000000000, 0.000000000000000000, 1.000000000000000000 ) ) ;
#3965 = STYLED_ITEM ( 'NONE', ( #12384 ), #6282 ) ;
#3966 = CARTESIAN_POINT ( 'NONE',  ( -79.99999999999995737, 316.7545334744432921, 155.1946179577816167 ) ) ;
#3967 = VERTEX_POINT ( 'NONE', #13503 ) ;
#3968 = CARTESIAN_POINT ( 'NONE',  ( 503.8334540492693918, 191.8198460455371333, 24.99421986894476078 ) ) ;
#3969 = EDGE_CURVE ( 'NONE', #19482, #72, #18223, .T. ) ;
#3970 = DIRECTION ( 'NONE',  ( 1.000000000000000000, 9.815121534730717399E-17, -0.000000000000000000 ) ) ;
#3971 = DIRECTION ( 'NONE',  ( 0.000000000000000000, 0.000000000000000000, 1.000000000000000000 ) ) ;
#3972 = CARTESIAN_POINT ( 'NONE',  ( -23.00000000000002487, 10.00000000000000000, -31.00000000000003553 ) ) ;
#3973 = ORIENTED_EDGE ( 'NONE', *, *, #20054, .T. ) ;
#3974 = EDGE_LOOP ( 'NONE', ( #17450, #12473, #9773, #12802 ) ) ;
#3975 = ADVANCED_FACE ( 'NONE', ( #989 ), #7314, .T. ) ;
#3976 = ORIENTED_EDGE ( 'NONE', *, *, #7986, .F. ) ;
#3977 = CIRCLE ( 'NONE', #8263, 1.800000000000000266 ) ;
#3978 =( GEOMETRIC_REPRESENTATION_CONTEXT ( 3 ) GLOBAL_UNCERTAINTY_ASSIGNED_CONTEXT ( ( #1023 ) ) GLOBAL_UNIT_ASSIGNED_CONTEXT ( ( #15714, #8270, #17642 ) ) REPRESENTATION_CONTEXT ( 'NONE', 'WORKASPACE' ) );
#3979 = VERTEX_POINT ( 'NONE', #15458 ) ;
#3980 = VERTEX_POINT ( 'NONE', #3068 ) ;
#3981 = LINE ( 'NONE', #3788, #9429 ) ;
#3982 = ORIENTED_EDGE ( 'NONE', *, *, #17986, .T. ) ;
#3983 = ADVANCED_FACE ( 'NONE', ( #12247 ), #13708, .F. ) ;
#3984 = LINE ( 'NONE', #15019, #3632 ) ;
#3985 = DIRECTION ( 'NONE',  ( 0.000000000000000000, 0.000000000000000000, -1.000000000000000000 ) ) ;
#3986 = EDGE_CURVE ( 'NONE', #3644, #12074, #10711, .T. ) ;
#3987 = CARTESIAN_POINT ( 'NONE',  ( 0.4913551399758951943, 139.7902036804299826, 489.4365304495848363 ) ) ;
#3988 = CARTESIAN_POINT ( 'NONE',  ( 463.8334540492693350, 191.8198460455371333, 71.76606011801538898 ) ) ;
#3989 = DIRECTION ( 'NONE',  ( -0.000000000000000000, -1.000000000000000000, 0.000000000000000000 ) ) ;
#3990 = PRESENTATION_LAYER_ASSIGNMENT (  '', '', ( #4981 ) ) ;
#3991 = CARTESIAN_POINT ( 'NONE',  ( 0.000000000000000000, 316.7545334744432353, 0.000000000000000000 ) ) ;
#3992 = STYLED_ITEM ( 'NONE', ( #2644 ), #17431 ) ;
#3993 = LINE ( 'NONE', #2846, #7748 ) ;
#3994 = AXIS2_PLACEMENT_3D ( 'NONE', #6408, #11128, #3297 ) ;
#3995 =( NAMED_UNIT ( * ) SI_UNIT ( $, .STERADIAN. ) SOLID_ANGLE_UNIT ( ) );
#3996 = CARTESIAN_POINT ( 'NONE',  ( -20.99999999999999645, 19.00000000000000000, -35.00000000000000711 ) ) ;
#3997 = UNCERTAINTY_MEASURE_WITH_UNIT (LENGTH_MEASURE( 1.000000000000000082E-05 ), #9155, 'distance_accuracy_value', 'NONE');
#3998 = CARTESIAN_POINT ( 'NONE',  ( 31.00000000000000000, 11.00000000000000000, 30.99999999999999289 ) ) ;
#3999 = DIRECTION ( 'NONE',  ( -1.000000000000000000, 0.000000000000000000, 0.000000000000000000 ) ) ;
#4000 = ORIENTED_EDGE ( 'NONE', *, *, #15809, .T. ) ;
#4001 = CARTESIAN_POINT ( 'NONE',  ( 35.00000000000000711, 8.000000000000000000, 20.99999999999999289 ) ) ;
#4002 = ORIENTED_EDGE ( 'NONE', *, *, #12942, .T. ) ;
#4003 = ORIENTED_EDGE ( 'NONE', *, *, #12093, .T. ) ;
#4005 = ORIENTED_EDGE ( 'NONE', *, *, #8600, .F. ) ;
#4004 = ADVANCED_FACE ( 'NONE', ( #17008 ), #2863, .F. ) ;
#4006 = DIRECTION ( 'NONE',  ( 0.000000000000000000, 0.000000000000000000, -1.000000000000000000 ) ) ;
#4007 = DIRECTION ( 'NONE',  ( 1.000000000000000000, 0.000000000000000000, 0.000000000000000000 ) ) ;
#4008 = AXIS2_PLACEMENT_3D ( 'NONE', #8512, #14797, #17992 ) ;
#4009 = SURFACE_STYLE_FILL_AREA ( #6826 ) ;
#4010 = DIRECTION ( 'NONE',  ( 3.328238341717372086E-14, 0.000000000000000000, -1.000000000000000000 ) ) ;
#4011 = CARTESIAN_POINT ( 'NONE',  ( -22.99999999999999645, 0.000000000000000000, 37.00000000000002132 ) ) ;
#4012 = PRESENTATION_STYLE_ASSIGNMENT (( #811 ) ) ;
#4013 = DIRECTION ( 'NONE',  ( 1.000000000000000000, 0.000000000000000000, 0.000000000000000000 ) ) ;
#4014 = FACE_OUTER_BOUND ( 'NONE', #4943, .T. ) ;
#4015 =( NAMED_UNIT ( * ) PLANE_ANGLE_UNIT ( ) SI_UNIT ( $, .RADIAN. ) );
#4016 = DIRECTION ( 'NONE',  ( -1.000000000000000000, 0.000000000000000000, 0.000000000000000000 ) ) ;
#4017 = CARTESIAN_POINT ( 'NONE',  ( -3.000000000000000000, 41.00000000000000711, 6.000000000000000000 ) ) ;
#4018 = LINE ( 'NONE', #5375, #12005 ) ;
#4019 = DIRECTION ( 'NONE',  ( 9.815121534730717399E-17, -1.000000000000000000, -0.000000000000000000 ) ) ;
#4020 = CIRCLE ( 'NONE', #7318, 10.00000000000000888 ) ;
#4021 = CIRCLE ( 'NONE', #5340, 8.999999999999952038 ) ;
#4022 = EDGE_LOOP ( 'NONE', ( #10564, #16560, #11147, #12078 ) ) ;
#4023 = ORIENTED_EDGE ( 'NONE', *, *, #17792, .T. ) ;
#4024 = AXIS2_PLACEMENT_3D ( 'NONE', #16880, #15543, #19939 ) ;
#4025 =( GEOMETRIC_REPRESENTATION_CONTEXT ( 3 ) GLOBAL_UNCERTAINTY_ASSIGNED_CONTEXT ( ( #426 ) ) GLOBAL_UNIT_ASSIGNED_CONTEXT ( ( #10471, #13865, #13678 ) ) REPRESENTATION_CONTEXT ( 'NONE', 'WORKASPACE' ) );
#4026 = CARTESIAN_POINT ( 'NONE',  ( 178.4893729001365728, 113.1299228374914918, 29.36128450348865471 ) ) ;
#4027 = ORIENTED_EDGE ( 'NONE', *, *, #14734, .T. ) ;
#4028 = EDGE_LOOP ( 'NONE', ( #18653, #1880, #861, #19417 ) ) ;
#4029 = EDGE_LOOP ( 'NONE', ( #12026, #18408, #16100, #6933 ) ) ;
#4030 =( NAMED_UNIT ( * ) SI_UNIT ( $, .STERADIAN. ) SOLID_ANGLE_UNIT ( ) );
#4031 = CARTESIAN_POINT ( 'NONE',  ( 19.99999999999995381, 0.000000000000000000, -36.99999999999999289 ) ) ;
#4032 =( GEOMETRIC_REPRESENTATION_CONTEXT ( 3 ) GLOBAL_UNCERTAINTY_ASSIGNED_CONTEXT ( ( #833 ) ) GLOBAL_UNIT_ASSIGNED_CONTEXT ( ( #11594, #10060, #14698 ) ) REPRESENTATION_CONTEXT ( 'NONE', 'WORKASPACE' ) );
#4033 = AXIS2_PLACEMENT_3D ( 'NONE', #19731, #882, #1173 ) ;
#4034 = VECTOR ( 'NONE', #6878, 1000.000000000000000 ) ;
#4035 = DIRECTION ( 'NONE',  ( 0.000000000000000000, 1.000000000000000000, 0.000000000000000000 ) ) ;
#4036 = DIRECTION ( 'NONE',  ( 0.000000000000000000, 1.000000000000000000, 0.000000000000000000 ) ) ;
#4037 = LINE ( 'NONE', #14972, #16310 ) ;
#4038 = EDGE_CURVE ( 'NONE', #4273, #15658, #12103, .T. ) ;
#4039 = LINE ( 'NONE', #10323, #11296 ) ;
#4040 = VECTOR ( 'NONE', #9945, 1000.000000000000000 ) ;
#4041 = SURFACE_STYLE_FILL_AREA ( #4160 ) ;
#4042 = DIRECTION ( 'NONE',  ( -0.000000000000000000, -0.000000000000000000, 1.000000000000000000 ) ) ;
#4043 = CARTESIAN_POINT ( 'NONE',  ( 1.574999999999999956, 0.000000000000000000, 0.000000000000000000 ) ) ;
#4044 = AXIS2_PLACEMENT_3D ( 'NONE', #19003, #8907, #6028 ) ;
#4045 = FACE_OUTER_BOUND ( 'NONE', #2081, .T. ) ;
#4046 = VECTOR ( 'NONE', #3470, 1000.000000000000000 ) ;
#4047 = ORIENTED_EDGE ( 'NONE', *, *, #20246, .T. ) ;
#4048 = PRESENTATION_LAYER_ASSIGNMENT (  '', '', ( #8647 ) ) ;
#4049 = LINE ( 'NONE', #5589, #451 ) ;
#4050 = CIRCLE ( 'NONE', #17523, 35.00000000000000711 ) ;
#4051 = VECTOR ( 'NONE', #16879, 1000.000000000000000 ) ;
#4052 = ORIENTED_EDGE ( 'NONE', *, *, #13580, .T. ) ;
#4053 = ADVANCED_FACE ( 'NONE', ( #1394 ), #14008, .F. ) ;
#4054 = SHAPE_REPRESENTATION ( 'Part14', ( #2741 ), #5024 ) ;
#4055 = VECTOR ( 'NONE', #16109, 1000.000000000000000 ) ;
#4056 = EDGE_LOOP ( 'NONE', ( #6896, #4654 ) ) ;
#4057 = CIRCLE ( 'NONE', #19833, 10.00000000000000888 ) ;
#4058 = DIRECTION ( 'NONE',  ( -6.120180426682197225E-17, 0.6235460666509320404, -0.7817866094812263578 ) ) ;
#4059 = CARTESIAN_POINT ( 'NONE',  ( 133.4893729001365443, 123.1299228374914634, 79.58252780074349175 ) ) ;
#4060 = VERTEX_POINT ( 'NONE', #4624 ) ;
#4061 = CARTESIAN_POINT ( 'NONE',  ( 1.224999999999999867, 15.25000000000000000, 0.000000000000000000 ) ) ;
#4062 = DIRECTION ( 'NONE',  ( 0.000000000000000000, 0.000000000000000000, 1.000000000000000000 ) ) ;
#4063 = LINE ( 'NONE', #4181, #12271 ) ;
#4064 = DIRECTION ( 'NONE',  ( 0.000000000000000000, 0.000000000000000000, -1.000000000000000000 ) ) ;
#4065 = STYLED_ITEM ( 'NONE', ( #3411 ), #14169 ) ;
#4066 = STYLED_ITEM ( 'NONE', ( #5714 ), #18929 ) ;
#4067 = CIRCLE ( 'NONE', #19844, 5.000000000000004441 ) ;
#4068 = FACE_OUTER_BOUND ( 'NONE', #9416, .T. ) ;
#4069 = CARTESIAN_POINT ( 'NONE',  ( 0.000000000000000000, 66.00000000000000000, -5.741599279633704455E-16 ) ) ;
#4070 = EDGE_CURVE ( 'NONE', #11158, #18080, #17189, .T. ) ;
#4071 = LINE ( 'NONE', #5516, #12683 ) ;
#4072 = ORIENTED_EDGE ( 'NONE', *, *, #13156, .T. ) ;
#4073 = PLANE ( 'NONE',  #280 ) ;
#4074 = FILL_AREA_STYLE ('',( #20008 ) ) ;
#4075 = FACE_OUTER_BOUND ( 'NONE', #18435, .T. ) ;
#4076 = AXIS2_PLACEMENT_3D ( 'NONE', #9326, #148, #6455 ) ;
#4077 = ORIENTED_EDGE ( 'NONE', *, *, #5833, .F. ) ;
#4078 = EDGE_CURVE ( 'NONE', #18534, #8487, #15772, .T. ) ;
#4079 = FACE_OUTER_BOUND ( 'NONE', #13664, .T. ) ;
#4080 =( GEOMETRIC_REPRESENTATION_CONTEXT ( 3 ) GLOBAL_UNCERTAINTY_ASSIGNED_CONTEXT ( ( #13586 ) ) GLOBAL_UNIT_ASSIGNED_CONTEXT ( ( #1262, #18399, #8838 ) ) REPRESENTATION_CONTEXT ( 'NONE', 'WORKASPACE' ) );
#4081 = VERTEX_POINT ( 'NONE', #282 ) ;
#4082 = ORIENTED_EDGE ( 'NONE', *, *, #16098, .F. ) ;
#4083 = ORIENTED_EDGE ( 'NONE', *, *, #9103, .F. ) ;
#4084 = AXIS2_PLACEMENT_3D ( 'NONE', #16286, #3594, #17484 ) ;
#4085 = CIRCLE ( 'NONE', #5728, 18.49999999999998934 ) ;
#4086 = VECTOR ( 'NONE', #16898, 1000.000000000000000 ) ;
#4087 = DIRECTION ( 'NONE',  ( -1.000000000000000000, -9.815121534730717399E-17, 0.000000000000000000 ) ) ;
#4088 = VECTOR ( 'NONE', #9581, 1000.000000000000000 ) ;
#4089 = ORIENTED_EDGE ( 'NONE', *, *, #15477, .T. ) ;
#4090 = EDGE_CURVE ( 'NONE', #9868, #2143, #15745, .T. ) ;
#4091 = DIRECTION ( 'NONE',  ( -3.854941057726253874E-16, 0.000000000000000000, -1.000000000000000000 ) ) ;
#4092 = ORIENTED_EDGE ( 'NONE', *, *, #11662, .F. ) ;
#4093 = DIRECTION ( 'NONE',  ( -1.000000000000000000, 0.000000000000000000, -0.000000000000000000 ) ) ;
#4094 = FACE_OUTER_BOUND ( 'NONE', #3399, .T. ) ;
#4095 = STYLED_ITEM ( 'NONE', ( #11537 ), #538 ) ;
#4096 = CARTESIAN_POINT ( 'NONE',  ( 111.4893729001366012, 127.7247684487574304, 250.0000000000000000 ) ) ;
#4097 = CARTESIAN_POINT ( 'NONE',  ( 0.000000000000000000, 141.3905724437643414, 503.0282008302663144 ) ) ;
#4098 = CARTESIAN_POINT ( 'NONE',  ( 0.4533632002511213122, 138.8714365591661704, 489.4163574291068812 ) ) ;
#4099 = EDGE_CURVE ( 'NONE', #3482, #1964, #12672, .T. ) ;
#4100 = CARTESIAN_POINT ( 'NONE',  ( 1.181929469892549101, 138.7545334744432637, 491.0690926367356042 ) ) ;
#4101 = STYLED_ITEM ( 'NONE', ( #5826 ), #12671 ) ;
#4102 = VECTOR ( 'NONE', #522, 1000.000000000000000 ) ;
#4103 = PLANE ( 'NONE',  #11628 ) ;
#4104 = CARTESIAN_POINT ( 'NONE',  ( -31.00000000000000000, 11.00000000000000000, 30.99999999999999289 ) ) ;
#4105 = DIRECTION ( 'NONE',  ( -0.000000000000000000, 1.000000000000000000, 0.000000000000000000 ) ) ;
#4106 = COLOUR_RGB ( '', 0.31764706, 0.68627451, 0.89019608) ;
#4107 = DIRECTION ( 'NONE',  ( 0.000000000000000000, 0.000000000000000000, -1.000000000000000000 ) ) ;
#4108 = EDGE_CURVE ( 'NONE', #8200, #16217, #14200, .T. ) ;
#4109 = CARTESIAN_POINT ( 'NONE',  ( -37.00000000000000711, 6.000000000000000000, -18.00000000000000355 ) ) ;
#4110 = CARTESIAN_POINT ( 'NONE',  ( 0.000000000000000000, 219.7545334744432921, 515.1946179577817020 ) ) ;
#4111 = VERTEX_POINT ( 'NONE', #11017 ) ;
#4112 = ADVANCED_FACE ( 'NONE', ( #17392 ), #18501, .F. ) ;
#4113 = MECHANICAL_DESIGN_GEOMETRIC_PRESENTATION_REPRESENTATION (  '', ( #1439 ), #12675 ) ;
#4114 = VERTEX_POINT ( 'NONE', #19259 ) ;
#4115 = UNCERTAINTY_MEASURE_WITH_UNIT (LENGTH_MEASURE( 1.000000000000000082E-05 ), #17577, 'distance_accuracy_value', 'NONE');
#4116 = AXIS2_PLACEMENT_3D ( 'NONE', #225, #15717, #1640 ) ;
#4117 = EDGE_CURVE ( 'NONE', #5163, #140, #577, .T. ) ;
#4118 = ORIENTED_EDGE ( 'NONE', *, *, #7761, .T. ) ;
#4119 = ORIENTED_EDGE ( 'NONE', *, *, #11953, .T. ) ;
#4120 = ADVANCED_FACE ( 'NONE', ( #4839, #1603, #11112, #1712, #3498, #4933 ), #17485, .T. ) ;
#4121 = COLOUR_RGB ( '', 0.40784314, 0.44705882, 0.49803922) ;
#4122 =( GEOMETRIC_REPRESENTATION_CONTEXT ( 3 ) GLOBAL_UNCERTAINTY_ASSIGNED_CONTEXT ( ( #15265 ) ) GLOBAL_UNIT_ASSIGNED_CONTEXT ( ( #2905, #10853, #1552 ) ) REPRESENTATION_CONTEXT ( 'NONE', 'WORKASPACE' ) );
#4123 = CARTESIAN_POINT ( 'NONE',  ( 0.000000000000000000, 316.7545334744432353, 515.1946179577817020 ) ) ;
#4124 = STYLED_ITEM ( 'NONE', ( #9780 ), #15290 ) ;
#4125 = CARTESIAN_POINT ( 'NONE',  ( -37.00000000000000000, 68.00000000000000000, 23.00000000000000355 ) ) ;
#4126 = CARTESIAN_POINT ( 'NONE',  ( 25.99999999999999645, 68.00000000000000000, 40.00000000000002132 ) ) ;
#4127 = AXIS2_PLACEMENT_3D ( 'NONE', #702, #5937, #9028 ) ;
#4128 =( LENGTH_UNIT ( ) NAMED_UNIT ( * ) SI_UNIT ( .MILLI., .METRE. ) );
#4129 = DIRECTION ( 'NONE',  ( 1.000000000000000000, -0.000000000000000000, -0.000000000000000000 ) ) ;
#4130 = DIRECTION ( 'NONE',  ( 0.000000000000000000, 0.000000000000000000, -1.000000000000000000 ) ) ;
#4131 = CIRCLE ( 'NONE', #14313, 10.00000000000000888 ) ;
#4132 = DIRECTION ( 'NONE',  ( 1.000000000000000000, 0.000000000000000000, 3.328238341717372086E-14 ) ) ;
#4133 =( NAMED_UNIT ( * ) SI_UNIT ( $, .STERADIAN. ) SOLID_ANGLE_UNIT ( ) );
#4134 = AXIS2_PLACEMENT_3D ( 'NONE', #650, #9841, #8411 ) ;
#4135 = CARTESIAN_POINT ( 'NONE',  ( 22.99999999999998224, 10.00000000000000000, -31.00000000000003197 ) ) ;
#4136 = VECTOR ( 'NONE', #13790, 1000.000000000000000 ) ;
#4137 = DIRECTION ( 'NONE',  ( 9.815121534730717399E-17, -1.000000000000000000, 0.000000000000000000 ) ) ;
#4138 = FILL_AREA_STYLE ('',( #2665 ) ) ;
#4139 = LINE ( 'NONE', #8949, #5622 ) ;
#4140 = CARTESIAN_POINT ( 'NONE',  ( -79.99999999999995737, 216.7545334744432921, 501.8237260975782874 ) ) ;
#4141 = CARTESIAN_POINT ( 'NONE',  ( 10.00000000000000000, 341.0487089519837696, -115.0000000000032969 ) ) ;
#4142 = LINE ( 'NONE', #15053, #10343 ) ;
#4143 = VECTOR ( 'NONE', #9536, 1000.000000000000114 ) ;
#4144 = CIRCLE ( 'NONE', #8423, 9.000000000000007105 ) ;
#4145 = EDGE_CURVE ( 'NONE', #10045, #12099, #9662, .T. ) ;
#4146 = VERTEX_POINT ( 'NONE', #11425 ) ;
#4147 = ORIENTED_EDGE ( 'NONE', *, *, #16565, .T. ) ;
#4148 = EDGE_CURVE ( 'NONE', #9009, #11794, #3884, .T. ) ;
#4149 = DIRECTION ( 'NONE',  ( -1.197852309262419498E-15, 1.000000000000000000, 0.000000000000000000 ) ) ;
#4150 = VERTEX_POINT ( 'NONE', #14406 ) ;
#4151 = ORIENTED_EDGE ( 'NONE', *, *, #11019, .T. ) ;
#4152 = DIRECTION ( 'NONE',  ( 0.000000000000000000, 0.000000000000000000, -1.000000000000000000 ) ) ;
#4153 = EDGE_CURVE ( 'NONE', #8580, #3628, #13125, .T. ) ;
#4154 = DIRECTION ( 'NONE',  ( -1.000000000000000000, 0.000000000000000000, 0.000000000000000000 ) ) ;
#4155 = UNCERTAINTY_MEASURE_WITH_UNIT (LENGTH_MEASURE( 1.000000000000000082E-05 ), #15597, 'distance_accuracy_value', 'NONE');
#4156 = DIRECTION ( 'NONE',  ( 1.000000000000000000, 5.889072920838430686E-16, -0.000000000000000000 ) ) ;
#4157 = DIRECTION ( 'NONE',  ( 0.000000000000000000, 0.000000000000000000, 1.000000000000000000 ) ) ;
#4158 = DIRECTION ( 'NONE',  ( 1.000000000000000000, 0.000000000000000000, 0.000000000000000000 ) ) ;
#4159 = PLANE ( 'NONE',  #8986 ) ;
#4160 = FILL_AREA_STYLE ('',( #18136 ) ) ;
#4161 = CARTESIAN_POINT ( 'NONE',  ( 34.00000000000002842, 0.000000000000000000, 31.00000000000000000 ) ) ;
#4162 =( NAMED_UNIT ( * ) SI_UNIT ( $, .STERADIAN. ) SOLID_ANGLE_UNIT ( ) );
#4163 = CARTESIAN_POINT ( 'NONE',  ( -80.46961127677876391, 138.7756291458123883, 490.4424144462261097 ) ) ;
#4164 = DIRECTION ( 'NONE',  ( 0.000000000000000000, 0.000000000000000000, -1.000000000000000000 ) ) ;
#4165 = ORIENTED_EDGE ( 'NONE', *, *, #19544, .T. ) ;
#4166 = DIRECTION ( 'NONE',  ( 1.000000000000000000, 0.000000000000000000, 0.000000000000000000 ) ) ;
#4167 = CARTESIAN_POINT ( 'NONE',  ( 108.9893729001366154, 131.2883416677199193, 282.8521325859589979 ) ) ;
#4168 = LINE ( 'NONE', #10333, #10332 ) ;
#4169 = PRESENTATION_LAYER_ASSIGNMENT (  '', '', ( #1139 ) ) ;
#4170 = VERTEX_POINT ( 'NONE', #8023 ) ;
#4171 = EDGE_CURVE ( 'NONE', #15133, #19368, #7918, .T. ) ;
#4172 = EDGE_LOOP ( 'NONE', ( #2453, #8455 ) ) ;
#4173 = UNCERTAINTY_MEASURE_WITH_UNIT (LENGTH_MEASURE( 1.000000000000000082E-05 ), #17002, 'distance_accuracy_value', 'NONE');
#4174 = PRESENTATION_LAYER_ASSIGNMENT (  '', '', ( #851 ) ) ;
#4175 = VERTEX_POINT ( 'NONE', #188 ) ;
#4176 = DIRECTION ( 'NONE',  ( 0.000000000000000000, 0.000000000000000000, -1.000000000000000000 ) ) ;
#4177 = DIRECTION ( 'NONE',  ( 0.000000000000000000, 0.000000000000000000, 1.000000000000000000 ) ) ;
#4178 = UNCERTAINTY_MEASURE_WITH_UNIT (LENGTH_MEASURE( 1.000000000000000082E-05 ), #19450, 'distance_accuracy_value', 'NONE');
#4179 = STYLED_ITEM ( 'NONE', ( #801 ), #9578 ) ;
#4180 = ORIENTED_EDGE ( 'NONE', *, *, #7724, .T. ) ;
#4181 = CARTESIAN_POINT ( 'NONE',  ( -211.5106270998635409, 103.1299228374912360, 79.58252780074349175 ) ) ;
#4182 =( LENGTH_UNIT ( ) NAMED_UNIT ( * ) SI_UNIT ( .MILLI., .METRE. ) );
#4183 = CARTESIAN_POINT ( 'NONE',  ( 1.163414459189985485E-15, 66.00000000000000000, 9.500000000000000000 ) ) ;
#4184 = LINE ( 'NONE', #10450, #7504 ) ;
#4185 = SPHERICAL_SURFACE ( 'NONE', #9504, 1.000000000000000000 ) ;
#4186 = CARTESIAN_POINT ( 'NONE',  ( 0.000000000000000000, 139.4861549369088323, 500.2186618848270996 ) ) ;
#4187 = CARTESIAN_POINT ( 'NONE',  ( 82.88953019741013861, 167.9162550801369491, 245.0000000000000000 ) ) ;
#4188 = PRODUCT_CONTEXT ( 'NONE', #19331, 'mechanical' ) ;
#4189 = EDGE_LOOP ( 'NONE', ( #19742, #5236, #3125, #12932 ) ) ;
#4190 = VERTEX_POINT ( 'NONE', #12878 ) ;
#4191 = ORIENTED_EDGE ( 'NONE', *, *, #19435, .F. ) ;
#4192 = VERTEX_POINT ( 'NONE', #19135 ) ;
#4193 = ORIENTED_EDGE ( 'NONE', *, *, #20202, .T. ) ;
#4194 = CARTESIAN_POINT ( 'NONE',  ( -40.00000000000000711, 10.00000000000000000, -26.00000000000000000 ) ) ;
#4195 = EDGE_CURVE ( 'NONE', #2876, #13587, #11791, .T. ) ;
#4196 = EDGE_LOOP ( 'NONE', ( #12377, #2646 ) ) ;
#4197 = CARTESIAN_POINT ( 'NONE',  ( 0.000000000000000000, 0.000000000000000000, -135.0000000000000284 ) ) ;
#4198 = CARTESIAN_POINT ( 'NONE',  ( -211.5106270998635409, 123.1299228374912644, 170.4174721992565082 ) ) ;
#4199 = ORIENTED_EDGE ( 'NONE', *, *, #2040, .T. ) ;
#4200 = SURFACE_STYLE_USAGE ( .BOTH. , #9128 ) ;
#4201 = CARTESIAN_POINT ( 'NONE',  ( -40.00000000000000711, 10.00000000000000000, 26.00000000000000000 ) ) ;
#4202 = VECTOR ( 'NONE', #10410, 1000.000000000000000 ) ;
#4203 = CARTESIAN_POINT ( 'NONE',  ( -37.00000000000000711, 10.00000000000000000, 23.00000000000000000 ) ) ;
#4204 = CARTESIAN_POINT ( 'NONE',  ( 493.8117674897343363, 214.2156642432025251, 245.0000000000000000 ) ) ;
#4205 = FACE_OUTER_BOUND ( 'NONE', #91, .T. ) ;
#4206 = CARTESIAN_POINT ( 'NONE',  ( -21.00000000000002842, -20.00000000000000000, -32.49999999999999289 ) ) ;
#4207 = ADVANCED_FACE ( 'NONE', ( #1912 ), #8233, .F. ) ;
#4208 = SURFACE_STYLE_USAGE ( .BOTH. , #8742 ) ;
#4209 = DIRECTION ( 'NONE',  ( 0.000000000000000000, -1.000000000000000000, -7.137148015447440312E-15 ) ) ;
#4210 = DIRECTION ( 'NONE',  ( 1.000000000000000000, 0.000000000000000000, 0.000000000000000000 ) ) ;
#4211 = CARTESIAN_POINT ( 'NONE',  ( 25.99999999999996092, 0.000000000000000000, 40.00000000000000711 ) ) ;
#4212 = SURFACE_STYLE_USAGE ( .BOTH. , #970 ) ;
#4213 = ORIENTED_EDGE ( 'NONE', *, *, #2461, .T. ) ;
#4214 = AXIS2_PLACEMENT_3D ( 'NONE', #10170, #16477, #2327 ) ;
#4215 = LINE ( 'NONE', #12653, #18918 ) ;
#4216 = ORIENTED_EDGE ( 'NONE', *, *, #18347, .F. ) ;
#4217 = APPLICATION_CONTEXT ( 'automotive_design' ) ;
#4218 = EDGE_CURVE ( 'NONE', #17862, #10840, #15080, .T. ) ;
#4219 = VERTEX_POINT ( 'NONE', #8740 ) ;
#4220 = EDGE_CURVE ( 'NONE', #6120, #715, #19983, .T. ) ;
#4221 = ORIENTED_EDGE ( 'NONE', *, *, #1287, .F. ) ;
#4222 = CARTESIAN_POINT ( 'NONE',  ( -78.99999999999995737, 146.1184945051221575, 507.7561228916242158 ) ) ;
#4223 = LINE ( 'NONE', #2237, #17442 ) ;
#4224 = ADVANCED_FACE ( 'NONE', ( #19433 ), #16688, .T. ) ;
#4225 = CARTESIAN_POINT ( 'NONE',  ( 111.4893729001366012, 127.7247684487574588, 357.7985149490353933 ) ) ;
#4226 = EDGE_CURVE ( 'NONE', #1663, #10340, #10466, .T. ) ;
#4227 = FACE_OUTER_BOUND ( 'NONE', #1660, .T. ) ;
#4228 = AXIS2_PLACEMENT_3D ( 'NONE', #2222, #17798, #588 ) ;
#4229 =( LENGTH_UNIT ( ) NAMED_UNIT ( * ) SI_UNIT ( .MILLI., .METRE. ) );
#4230 = DIRECTION ( 'NONE',  ( 1.000000000000000000, 9.815121534730717399E-17, -0.000000000000000000 ) ) ;
#4231 = CARTESIAN_POINT ( 'NONE',  ( 25.99999999999997868, 0.000000000000000000, -39.99999999999999289 ) ) ;
#4232 = FACE_OUTER_BOUND ( 'NONE', #16219, .T. ) ;
#4233 = CARTESIAN_POINT ( 'NONE',  ( -26.00000000000002132, 10.00000000000000000, 40.00000000000000711 ) ) ;
#4234 = DIRECTION ( 'NONE',  ( 0.000000000000000000, 1.000000000000000000, 0.000000000000000000 ) ) ;
#4235 = DIRECTION ( 'NONE',  ( 0.000000000000000000, 0.000000000000000000, -1.000000000000000000 ) ) ;
#4236 = EDGE_CURVE ( 'NONE', #20287, #4620, #12780, .T. ) ;
#4237 = ORIENTED_EDGE ( 'NONE', *, *, #10751, .T. ) ;
#4238 = EDGE_CURVE ( 'NONE', #13587, #19445, #780, .T. ) ;
#4239 =( GEOMETRIC_REPRESENTATION_CONTEXT ( 3 ) GLOBAL_UNCERTAINTY_ASSIGNED_CONTEXT ( ( #6865 ) ) GLOBAL_UNIT_ASSIGNED_CONTEXT ( ( #2202, #5615, #2518 ) ) REPRESENTATION_CONTEXT ( 'NONE', 'WORKASPACE' ) );
#4240 = FACE_BOUND ( 'NONE', #6707, .T. ) ;
#4241 = EDGE_LOOP ( 'NONE', ( #3864, #4523 ) ) ;
#4242 = ORIENTED_EDGE ( 'NONE', *, *, #3881, .F. ) ;
#4243 = LINE ( 'NONE', #8295, #8764 ) ;
#4244 = LINE ( 'NONE', #18441, #16280 ) ;
#4245 = PLANE ( 'NONE',  #2331 ) ;
#4246 = DIRECTION ( 'NONE',  ( 1.000000000000000000, 0.000000000000000000, 0.000000000000000000 ) ) ;
#4247 = CARTESIAN_POINT ( 'NONE',  ( -3.000000000000003109, 66.00000000000000000, 9.013878188659973034 ) ) ;
#4248 = DIRECTION ( 'NONE',  ( 1.000000000000000000, 0.000000000000000000, 0.000000000000000000 ) ) ;
#4249 = PLANE ( 'NONE',  #7661 ) ;
#4250 = ADVANCED_FACE ( 'NONE', ( #3896 ), #7104, .T. ) ;
#4251 = FACE_OUTER_BOUND ( 'NONE', #1514, .T. ) ;
#4252 = FACE_OUTER_BOUND ( 'NONE', #9076, .T. ) ;
#4253 = VECTOR ( 'NONE', #2270, 1000.000000000000000 ) ;
#4254 = ORIENTED_EDGE ( 'NONE', *, *, #2947, .F. ) ;
#4255 = PRESENTATION_STYLE_ASSIGNMENT (( #1315 ) ) ;
#4256 = SURFACE_STYLE_FILL_AREA ( #5809 ) ;
#4257 = ORIENTED_EDGE ( 'NONE', *, *, #18795, .F. ) ;
#4258 = STYLED_ITEM ( 'NONE', ( #2139 ), #16193 ) ;
#4259 = COLOUR_RGB ( '', 0.72549020, 0.75294118, 0.79215686) ;
#4260 = AXIS2_PLACEMENT_3D ( 'NONE', #19732, #5755, #5644 ) ;
#4262 = VERTEX_POINT ( 'NONE', #14719 ) ;
#4261 = PRESENTATION_LAYER_ASSIGNMENT (  '', '', ( #9189 ) ) ;
#4263 = EDGE_CURVE ( 'NONE', #9458, #20152, #18196, .T. ) ;
#4264 = CARTESIAN_POINT ( 'NONE',  ( 0.000000000000000000, 0.000000000000000000, 0.000000000000000000 ) ) ;
#4265 = FILL_AREA_STYLE ('',( #18361 ) ) ;
#4266 = VERTEX_POINT ( 'NONE', #4100 ) ;
#4267 = CARTESIAN_POINT ( 'NONE',  ( -37.00000000000000711, 0.000000000000000000, -23.00000000000000000 ) ) ;
#4268 =( NAMED_UNIT ( * ) PLANE_ANGLE_UNIT ( ) SI_UNIT ( $, .RADIAN. ) );
#4269 =( NAMED_UNIT ( * ) SI_UNIT ( $, .STERADIAN. ) SOLID_ANGLE_UNIT ( ) );
#4270 = CARTESIAN_POINT ( 'NONE',  ( -31.00000000000002842, 68.00000000000000000, -25.99999999999999645 ) ) ;
#4271 =( LENGTH_UNIT ( ) NAMED_UNIT ( * ) SI_UNIT ( .MILLI., .METRE. ) );
#4272 = SURFACE_SIDE_STYLE ('',( #7177 ) ) ;
#4273 = VERTEX_POINT ( 'NONE', #6808 ) ;
#4274 = DIRECTION ( 'NONE',  ( 0.000000000000000000, 1.000000000000000000, 0.000000000000000000 ) ) ;
#4275 = DIRECTION ( 'NONE',  ( 0.000000000000000000, 1.000000000000000000, 0.000000000000000000 ) ) ;
#4276 = CIRCLE ( 'NONE', #2616, 2.500000000000002220 ) ;
#4277 = APPLICATION_PROTOCOL_DEFINITION ( 'draft international standard', 'automotive_design', 1998, #11576 ) ;
#4278 = AXIS2_PLACEMENT_3D ( 'NONE', #19130, #8132, #4834 ) ;
#4279 = VECTOR ( 'NONE', #3660, 1000.000000000000000 ) ;
#4280 = ORIENTED_EDGE ( 'NONE', *, *, #6579, .T. ) ;
#4281 = ORIENTED_EDGE ( 'NONE', *, *, #10646, .T. ) ;
#4282 = VERTEX_POINT ( 'NONE', #18092 ) ;
#4283 = ORIENTED_EDGE ( 'NONE', *, *, #1258, .T. ) ;
#4284 = DIRECTION ( 'NONE',  ( -0.000000000000000000, -1.000000000000000000, -0.000000000000000000 ) ) ;
#4285 = VERTEX_POINT ( 'NONE', #5341 ) ;
#4286 = DIRECTION ( 'NONE',  ( -0.000000000000000000, 1.000000000000000000, -0.000000000000000000 ) ) ;
#4287 = AXIS2_PLACEMENT_3D ( 'NONE', #13654, #9004, #10152 ) ;
#4288 = VECTOR ( 'NONE', #10981, 1000.000000000000000 ) ;
#4289 =( NAMED_UNIT ( * ) SI_UNIT ( $, .STERADIAN. ) SOLID_ANGLE_UNIT ( ) );
#4290 = AXIS2_PLACEMENT_3D ( 'NONE', #7064, #13361, #11274 ) ;
#4291 = SURFACE_STYLE_USAGE ( .BOTH. , #7192 ) ;
#4292 =( LENGTH_UNIT ( ) NAMED_UNIT ( * ) SI_UNIT ( .MILLI., .METRE. ) );
#4293 = FACE_BOUND ( 'NONE', #11841, .T. ) ;
#4294 = EDGE_CURVE ( 'NONE', #3644, #16358, #5447, .T. ) ;
#4295 = DIRECTION ( 'NONE',  ( 1.000000000000000000, 0.000000000000000000, 0.000000000000000000 ) ) ;
#4296 = LINE ( 'NONE', #18305, #17708 ) ;
#4297 = LINE ( 'NONE', #10578, #403 ) ;
#4298 = DIRECTION ( 'NONE',  ( -0.000000000000000000, -1.000000000000000000, -0.000000000000000000 ) ) ;
#4299 = CARTESIAN_POINT ( 'NONE',  ( 30.90550859392666183, -37.11391548236649385, 66.87703344121200644 ) ) ;
#4300 = CARTESIAN_POINT ( 'NONE',  ( 30.99999999999995737, 3.000000000000000000, 31.00000000000000000 ) ) ;
#4301 = LINE ( 'NONE', #7405, #19461 ) ;
#4302 = ORIENTED_EDGE ( 'NONE', *, *, #1132, .F. ) ;
#4303 =( GEOMETRIC_REPRESENTATION_CONTEXT ( 3 ) GLOBAL_UNCERTAINTY_ASSIGNED_CONTEXT ( ( #19790 ) ) GLOBAL_UNIT_ASSIGNED_CONTEXT ( ( #13701, #18414, #12237 ) ) REPRESENTATION_CONTEXT ( 'NONE', 'WORKASPACE' ) );
#4304 = EDGE_CURVE ( 'NONE', #18104, #10793, #18021, .T. ) ;
#4305 = ORIENTED_EDGE ( 'NONE', *, *, #19432, .T. ) ;
#4306 = PRESENTATION_LAYER_ASSIGNMENT (  '', '', ( #11548 ) ) ;
#4307 = EDGE_LOOP ( 'NONE', ( #14630, #16766, #13754, #2454 ) ) ;
#4308 = EDGE_CURVE ( 'NONE', #19266, #6461, #19342, .T. ) ;
#4309 = DIRECTION ( 'NONE',  ( 2.135044278125301096E-16, -1.000000000000000000, 0.000000000000000000 ) ) ;
#4310 = ORIENTED_EDGE ( 'NONE', *, *, #18299, .F. ) ;
#4311 = CARTESIAN_POINT ( 'NONE',  ( 486.8117674897343363, 214.2156642432025251, 250.0000000000000000 ) ) ;
#4312 = CARTESIAN_POINT ( 'NONE',  ( 463.8334540492693350, 214.2156642432025251, 250.0000000000000000 ) ) ;
#4313 = ORIENTED_EDGE ( 'NONE', *, *, #839, .T. ) ;
#4314 = CARTESIAN_POINT ( 'NONE',  ( 463.8334540492693350, 134.2156642432025251, 0.000000000000000000 ) ) ;
#4315 = VECTOR ( 'NONE', #194, 1000.000000000000000 ) ;
#4316 = DIRECTION ( 'NONE',  ( -0.000000000000000000, -1.000000000000000000, 0.000000000000000000 ) ) ;
#4317 = CARTESIAN_POINT ( 'NONE',  ( 423.8334540492694487, 191.8198460455371333, 14.99421986894475012 ) ) ;
#4318 =( LENGTH_UNIT ( ) NAMED_UNIT ( * ) SI_UNIT ( .MILLI., .METRE. ) );
#4319 = FACE_OUTER_BOUND ( 'NONE', #8638, .T. ) ;
#4320 = DIRECTION ( 'NONE',  ( 0.000000000000000000, 1.000000000000000000, 0.000000000000000000 ) ) ;
#4321 = FILL_AREA_STYLE ('',( #991 ) ) ;
#4322 = FACE_OUTER_BOUND ( 'NONE', #10260, .T. ) ;
#4323 = ADVANCED_FACE ( 'NONE', ( #15024 ), #2132, .T. ) ;
#4324 = CARTESIAN_POINT ( 'NONE',  ( -41.50085094405407915, 159.0821755739672483, 510.3921618609452935 ) ) ;
#4325 = CARTESIAN_POINT ( 'NONE',  ( 30.99999999999999645, 0.000000000000000000, -25.99999999999999645 ) ) ;
#4326 = ORIENTED_EDGE ( 'NONE', *, *, #7264, .T. ) ;
#4327 = EDGE_CURVE ( 'NONE', #7832, #6379, #16582, .T. ) ;
#4328 = VECTOR ( 'NONE', #16695, 1000.000000000000000 ) ;
#4329 = ORIENTED_EDGE ( 'NONE', *, *, #12438, .T. ) ;
#4330 = ORIENTED_EDGE ( 'NONE', *, *, #15909, .T. ) ;
#4331 = DIRECTION ( 'NONE',  ( 0.000000000000000000, 0.000000000000000000, -1.000000000000000000 ) ) ;
#4332 = ORIENTED_EDGE ( 'NONE', *, *, #19452, .T. ) ;
#4333 = ORIENTED_EDGE ( 'NONE', *, *, #3714, .T. ) ;
#4334 =( NAMED_UNIT ( * ) PLANE_ANGLE_UNIT ( ) SI_UNIT ( $, .RADIAN. ) );
#4335 = EDGE_CURVE ( 'NONE', #11484, #19448, #16409, .T. ) ;
#4336 = DIRECTION ( 'NONE',  ( -0.000000000000000000, 0.000000000000000000, 1.000000000000000000 ) ) ;
#4337 = UNCERTAINTY_MEASURE_WITH_UNIT (LENGTH_MEASURE( 1.000000000000000082E-05 ), #19870, 'distance_accuracy_value', 'NONE');
#4338 = CARTESIAN_POINT ( 'NONE',  ( 78.48937290013661539, 80.91625508013694912, -97.94896630388704750 ) ) ;
#4339 = EDGE_CURVE ( 'NONE', #15180, #13028, #13283, .T. ) ;
#4340 = DIRECTION ( 'NONE',  ( -1.000000000000000000, 0.000000000000000000, -0.000000000000000000 ) ) ;
#4341 = DIRECTION ( 'NONE',  ( 1.000000000000000000, 0.000000000000000000, -0.000000000000000000 ) ) ;
#4342 = CARTESIAN_POINT ( 'NONE',  ( -31.00000000000003553, 19.00000000000000000, -21.00000000000000000 ) ) ;
#4343 = LINE ( 'NONE', #10830, #2725 ) ;
#4344 = CIRCLE ( 'NONE', #2685, 4.999999999999997335 ) ;
#4345 = LINE ( 'NONE', #4161, #3765 ) ;
#4346 = CARTESIAN_POINT ( 'NONE',  ( -79.99999999999995737, 140.4048636633015406, 500.8237260975782874 ) ) ;
#4347 = DIRECTION ( 'NONE',  ( -1.000000000000000000, 0.000000000000000000, 0.000000000000000000 ) ) ;
#4348 = EDGE_CURVE ( 'NONE', #6703, #4581, #7507, .T. ) ;
#4349 = VERTEX_POINT ( 'NONE', #7196 ) ;
#4350 =( NAMED_UNIT ( * ) PLANE_ANGLE_UNIT ( ) SI_UNIT ( $, .RADIAN. ) );
#4351 = CARTESIAN_POINT ( 'NONE',  ( 5.941205806953520074, 15.14120580695428764, 0.000000000000000000 ) ) ;
#4352 =( GEOMETRIC_REPRESENTATION_CONTEXT ( 3 ) GLOBAL_UNCERTAINTY_ASSIGNED_CONTEXT ( ( #8275 ) ) GLOBAL_UNIT_ASSIGNED_CONTEXT ( ( #17482, #9776, #6381 ) ) REPRESENTATION_CONTEXT ( 'NONE', 'WORKASPACE' ) );
#4353 = EDGE_CURVE ( 'NONE', #3066, #19421, #13394, .T. ) ;
#4354 = VERTEX_POINT ( 'NONE', #13483 ) ;
#4355 = AXIS2_PLACEMENT_3D ( 'NONE', #11164, #18688, #1467 ) ;
#4356 = CIRCLE ( 'NONE', #9967, 10.00000000000000888 ) ;
#4357 = EDGE_LOOP ( 'NONE', ( #15310, #1202 ) ) ;
#4358 = CARTESIAN_POINT ( 'NONE',  ( 463.8334540492693350, 134.2156642432025251, 250.0000000000000000 ) ) ;
#4359 = EDGE_LOOP ( 'NONE', ( #12032, #14328, #14087, #90 ) ) ;
#4360 = LINE ( 'NONE', #17235, #13686 ) ;
#4361 = AXIS2_PLACEMENT_3D ( 'NONE', #18254, #15276, #19990 ) ;
#4362 = CARTESIAN_POINT ( 'NONE',  ( -80.11724004894423956, 140.9328816482941420, 501.3369121427558639 ) ) ;
#4363 = DIRECTION ( 'NONE',  ( -1.000000000000000000, 0.000000000000000000, -0.000000000000000000 ) ) ;
#4364 = SURFACE_STYLE_FILL_AREA ( #18470 ) ;
#4365 = EDGE_LOOP ( 'NONE', ( #8882, #117, #14257, #11121 ) ) ;
#4366 = DIRECTION ( 'NONE',  ( 7.715811803773179210E-14, 0.000000000000000000, 1.000000000000000000 ) ) ;
#4367 = AXIS2_PLACEMENT_3D ( 'NONE', #5290, #6944, #13228 ) ;
#4368 = LINE ( 'NONE', #18284, #2090 ) ;
#4369 = APPLICATION_PROTOCOL_DEFINITION ( 'draft international standard', 'automotive_design', 1998, #14462 ) ;
#4370 = ORIENTED_EDGE ( 'NONE', *, *, #18854, .F. ) ;
#4371 = VERTEX_POINT ( 'NONE', #19726 ) ;
#4372 =( NAMED_UNIT ( * ) SI_UNIT ( $, .STERADIAN. ) SOLID_ANGLE_UNIT ( ) );
#4373 = AXIS2_PLACEMENT_3D ( 'NONE', #14880, #2606, #19607 ) ;
#4374 = EDGE_CURVE ( 'NONE', #20130, #8866, #1887, .T. ) ;
#4375 = ORIENTED_EDGE ( 'NONE', *, *, #6975, .T. ) ;
#4376 = ORIENTED_EDGE ( 'NONE', *, *, #4957, .F. ) ;
#4377 = VECTOR ( 'NONE', #9797, 1000.000000000000000 ) ;
#4378 = ORIENTED_EDGE ( 'NONE', *, *, #1935, .F. ) ;
#4379 = EDGE_CURVE ( 'NONE', #6860, #5413, #6050, .T. ) ;
#4380 = DIRECTION ( 'NONE',  ( 1.000000000000000000, 0.000000000000000000, -3.854941057726258312E-16 ) ) ;
#4381 = EDGE_LOOP ( 'NONE', ( #17015, #2008, #6143, #14107 ) ) ;
#4382 = DIRECTION ( 'NONE',  ( 0.000000000000000000, 0.000000000000000000, -1.000000000000000000 ) ) ;
#4383 = AXIS2_PLACEMENT_3D ( 'NONE', #14531, #10273, #520 ) ;
#4384 = CARTESIAN_POINT ( 'NONE',  ( 498.8334540492693918, 191.8198460455371333, 215.0057801310552179 ) ) ;
#4385 = DIRECTION ( 'NONE',  ( -1.000000000000000000, 0.000000000000000000, 3.854941057726249930E-16 ) ) ;
#4386 = DIRECTION ( 'NONE',  ( -9.815121534730717399E-17, 1.000000000000000000, 0.000000000000000000 ) ) ;
#4387 = DIRECTION ( 'NONE',  ( 0.000000000000000000, 0.000000000000000000, -1.000000000000000000 ) ) ;
#4388 = DIRECTION ( 'NONE',  ( 0.000000000000000000, 0.000000000000000000, 1.000000000000000000 ) ) ;
#4389 = CARTESIAN_POINT ( 'NONE',  ( -44.50085094405410757, 209.4098724938429541, 510.3921618609452935 ) ) ;
#4390 = VECTOR ( 'NONE', #13329, 1000.000000000000000 ) ;
#4391 = STYLED_ITEM ( 'NONE', ( #2766 ), #20192 ) ;
#4392 = LINE ( 'NONE', #5746, #18357 ) ;
#4393 = LINE ( 'NONE', #10272, #720 ) ;
#4394 = DIRECTION ( 'NONE',  ( -1.000000000000000000, -0.000000000000000000, -0.000000000000000000 ) ) ;
#4395 =( LENGTH_UNIT ( ) NAMED_UNIT ( * ) SI_UNIT ( .MILLI., .METRE. ) );
#4396 = DIRECTION ( 'NONE',  ( -0.000000000000000000, -1.000000000000000000, 0.000000000000000000 ) ) ;
#4397 = CARTESIAN_POINT ( 'NONE',  ( -18.00000000000001421, 6.000000000000000000, 36.00000000000000711 ) ) ;
#4398 = DIRECTION ( 'NONE',  ( -1.000000000000000000, 0.000000000000000000, 0.000000000000000000 ) ) ;
#4399 = STYLED_ITEM ( 'NONE', ( #9554 ), #12216 ) ;
#4400 = ORIENTED_EDGE ( 'NONE', *, *, #3489, .T. ) ;
#4401 = VECTOR ( 'NONE', #14700, 1000.000000000000000 ) ;
#4402 = VECTOR ( 'NONE', #11539, 1000.000000000000000 ) ;
#4403 = ORIENTED_EDGE ( 'NONE', *, *, #19626, .F. ) ;
#4404 = EDGE_LOOP ( 'NONE', ( #11295, #7039, #1416, #7783 ) ) ;
#4405 = VECTOR ( 'NONE', #7658, 1000.000000000000000 ) ;
#4406 = ADVANCED_FACE ( 'NONE', ( #5940 ), #12123, .T. ) ;
#4407 = STYLED_ITEM ( 'NONE', ( #19880 ), #239 ) ;
#4408 = EDGE_LOOP ( 'NONE', ( #8864, #15371 ) ) ;
#4409 = CARTESIAN_POINT ( 'NONE',  ( -80.31054232717158925, 138.7814785482270565, 490.3703103398013354 ) ) ;
#4410 = ORIENTED_EDGE ( 'NONE', *, *, #7619, .T. ) ;
#4411 = CARTESIAN_POINT ( 'NONE',  ( 0.000000000000000000, 372.8685141053778693, -83.18019484660869978 ) ) ;
#4412 = DIRECTION ( 'NONE',  ( -1.000000000000000000, -0.000000000000000000, -0.000000000000000000 ) ) ;
#4413 = ORIENTED_EDGE ( 'NONE', *, *, #1427, .T. ) ;
#4414 = COLOUR_RGB ( '', 0.08235294, 0.09019608, 0.10196078) ;
#4415 = VECTOR ( 'NONE', #17545, 1000.000000000000000 ) ;
#4416 = SURFACE_STYLE_USAGE ( .BOTH. , #18519 ) ;
#4417 = CARTESIAN_POINT ( 'NONE',  ( -31.00000000000000000, 19.00000000000000000, -31.00000000000000000 ) ) ;
#4418 = DIRECTION ( 'NONE',  ( 0.000000000000000000, 1.000000000000000000, 0.000000000000000000 ) ) ;
#4419 = VECTOR ( 'NONE', #2384, 1000.000000000000000 ) ;
#4420 = PRESENTATION_STYLE_ASSIGNMENT (( #8945 ) ) ;
#4421 = DIRECTION ( 'NONE',  ( 0.000000000000000000, 0.000000000000000000, 1.000000000000000000 ) ) ;
#4422 = CARTESIAN_POINT ( 'NONE',  ( -78.99999999999995737, 141.3905724437643698, 484.7051316060566819 ) ) ;
#4423 = SURFACE_SIDE_STYLE ('',( #15145 ) ) ;
#4424 = PRESENTATION_LAYER_ASSIGNMENT (  '', '', ( #10039 ) ) ;
#4425 = AXIS2_PLACEMENT_3D ( 'NONE', #10801, #17082, #2956 ) ;
#4426 = DIRECTION ( 'NONE',  ( 1.000000000000000000, 0.000000000000000000, 0.000000000000000000 ) ) ;
#4427 = COLOUR_RGB ( '', 0.09019608, 0.27058824, 0.51372549) ;
#4428 = EDGE_CURVE ( 'NONE', #4146, #3049, #10577, .T. ) ;
#4429 = AXIS2_PLACEMENT_3D ( 'NONE', #3229, #4880, #1963 ) ;
#4430 = VECTOR ( 'NONE', #5275, 1000.000000000000000 ) ;
#4431 = ORIENTED_EDGE ( 'NONE', *, *, #3213, .F. ) ;
#4432 = VECTOR ( 'NONE', #9502, 1000.000000000000000 ) ;
#4433 = ORIENTED_EDGE ( 'NONE', *, *, #1358, .F. ) ;
#4434 = CIRCLE ( 'NONE', #8061, 8.000000000000007105 ) ;
#4435 = LINE ( 'NONE', #9380, #133 ) ;
#4436 = ORIENTED_EDGE ( 'NONE', *, *, #9927, .T. ) ;
#4437 = EDGE_LOOP ( 'NONE', ( #15197, #4867, #11819, #2390 ) ) ;
#4438 = DIRECTION ( 'NONE',  ( 1.000000000000000000, 0.000000000000000000, 0.000000000000000000 ) ) ;
#4439 = AXIS2_PLACEMENT_3D ( 'NONE', #4197, #19928, #12115 ) ;
#4440 = EDGE_CURVE ( 'NONE', #20158, #17622, #17071, .T. ) ;
#4441 = CARTESIAN_POINT ( 'NONE',  ( -34.99999999999998579, -20.00000000000000000, 18.50000000000000355 ) ) ;
#4442 = VECTOR ( 'NONE', #2122, 1000.000000000000000 ) ;
#4443 = CARTESIAN_POINT ( 'NONE',  ( 53.48937290013659407, 0.000000000000000000, -97.94896630388704750 ) ) ;
#4444 = VECTOR ( 'NONE', #3181, 1000.000000000000000 ) ;
#4445 = PRESENTATION_STYLE_ASSIGNMENT (( #7744 ) ) ;
#4446 = CARTESIAN_POINT ( 'NONE',  ( 53.48937290013660828, 34.32473510485366575, -140.0000000000001137 ) ) ;
#4447 = PRODUCT_RELATED_PRODUCT_CATEGORY ( 'part', '', ( #11412 ) ) ;
#4448 = LINE ( 'NONE', #17111, #729 ) ;
#4449 = VECTOR ( 'NONE', #11783, 1000.000000000000000 ) ;
#4450 = VECTOR ( 'NONE', #17376, 1000.000000000000000 ) ;
#4451 = DIRECTION ( 'NONE',  ( 6.263247009234064878E-17, -0.6381222063396385646, 0.7699350945217602327 ) ) ;
#4452 = DIRECTION ( 'NONE',  ( 0.000000000000000000, -1.000000000000000000, -7.137148015447440312E-15 ) ) ;
#4453 = PRESENTATION_LAYER_ASSIGNMENT (  '', '', ( #823 ) ) ;
#4454 = EDGE_LOOP ( 'NONE', ( #17593, #13861 ) ) ;
#4455 = DIRECTION ( 'NONE',  ( 0.000000000000000000, 0.000000000000000000, -1.000000000000000000 ) ) ;
#4456 = EDGE_CURVE ( 'NONE', #17994, #3506, #964, .T. ) ;
#4457 = FACE_OUTER_BOUND ( 'NONE', #9214, .T. ) ;
#4458 = VECTOR ( 'NONE', #12815, 1000.000000000000000 ) ;
#4459 = ADVANCED_FACE ( 'NONE', ( #7693 ), #9133, .F. ) ;
#4460 = AXIS2_PLACEMENT_3D ( 'NONE', #7679, #19715, #5628 ) ;
#4461 = ORIENTED_EDGE ( 'NONE', *, *, #15018, .F. ) ;
#4462 = EDGE_CURVE ( 'NONE', #9184, #9751, #13769, .T. ) ;
#4463 = CARTESIAN_POINT ( 'NONE',  ( 153.4893729001366864, 113.1299228374914634, 220.6387154965113382 ) ) ;
#4464 = ORIENTED_EDGE ( 'NONE', *, *, #9786, .F. ) ;
#4465 = CARTESIAN_POINT ( 'NONE',  ( -23.00000000000002132, 10.00000000000000000, 37.00000000000000711 ) ) ;
#4466 = CARTESIAN_POINT ( 'NONE',  ( 53.48937290013658696, 119.5973956464515879, 322.0399576098686225 ) ) ;
#4467 = ORIENTED_EDGE ( 'NONE', *, *, #6541, .T. ) ;
#4468 = DIRECTION ( 'NONE',  ( 0.000000000000000000, 0.000000000000000000, -1.000000000000000000 ) ) ;
#4469 =( NAMED_UNIT ( * ) SI_UNIT ( $, .STERADIAN. ) SOLID_ANGLE_UNIT ( ) );
#4470 = AXIS2_PLACEMENT_3D ( 'NONE', #15483, #4341, #18545 ) ;
#4471 = CARTESIAN_POINT ( 'NONE',  ( 98.48937290013662960, 103.1299228374914208, 220.6387154965113382 ) ) ;
#4472 = EDGE_CURVE ( 'NONE', #3089, #12943, #4296, .T. ) ;
#4473 = AXIS2_PLACEMENT_3D ( 'NONE', #5260, #1929, #11125 ) ;
#4474 = DIRECTION ( 'NONE',  ( -1.445602896647339163E-16, 1.000000000000000000, 0.000000000000000000 ) ) ;
#4475 = EDGE_CURVE ( 'NONE', #14026, #20287, #4602, .T. ) ;
#4476 = PLANE ( 'NONE',  #16406 ) ;
#4477 = DIRECTION ( 'NONE',  ( -1.000000000000000000, 0.000000000000000000, -0.000000000000000000 ) ) ;
#4478 = FACE_OUTER_BOUND ( 'NONE', #16384, .T. ) ;
#4479 = ORIENTED_EDGE ( 'NONE', *, *, #7241, .F. ) ;
#4480 = CARTESIAN_POINT ( 'NONE',  ( 0.000000000000000000, 66.00000000000000000, -5.741599279633704455E-16 ) ) ;
#4481 = SURFACE_STYLE_USAGE ( .BOTH. , #18473 ) ;
#4482 = DIRECTION ( 'NONE',  ( 0.000000000000000000, -0.000000000000000000, 1.000000000000000000 ) ) ;
#4483 = PRODUCT_DEFINITION_SHAPE ( 'NONE', 'NONE',  #20387 ) ;
#4484 = VERTEX_POINT ( 'NONE', #15121 ) ;
#4485 = LINE ( 'NONE', #9210, #4677 ) ;
#4486 = EDGE_CURVE ( 'NONE', #13473, #8466, #4392, .T. ) ;
#4487 = ORIENTED_EDGE ( 'NONE', *, *, #5488, .F. ) ;
#4488 = ORIENTED_EDGE ( 'NONE', *, *, #16002, .T. ) ;
#4489 = AXIS2_PLACEMENT_3D ( 'NONE', #14738, #10103, #11854 ) ;
#4490 = ORIENTED_EDGE ( 'NONE', *, *, #16048, .F. ) ;
#4491 = AXIS2_PLACEMENT_3D ( 'NONE', #8538, #8642, #17918 ) ;
#4492 = DIRECTION ( 'NONE',  ( 1.000000000000000000, -0.000000000000000000, 0.000000000000000000 ) ) ;
#4493 = EDGE_CURVE ( 'NONE', #18122, #17418, #3900, .T. ) ;
#4494 = EDGE_LOOP ( 'NONE', ( #13326, #4721, #4743, #15683 ) ) ;
#4495 = LINE ( 'NONE', #10569, #13408 ) ;
#4496 = LINE ( 'NONE', #10775, #19848 ) ;
#4497 = PLANE ( 'NONE',  #8330 ) ;
#4498 = DIRECTION ( 'NONE',  ( 0.000000000000000000, 1.000000000000000000, 0.000000000000000000 ) ) ;
#4499 = LINE ( 'NONE', #9027, #9600 ) ;
#4500 = CARTESIAN_POINT ( 'NONE',  ( 2.999999999999996891, 60.00000000000000711, 9.013878188659974811 ) ) ;
#4501 = CYLINDRICAL_SURFACE ( 'NONE', #18075, 1.000000000000000888 ) ;
#4502 = SURFACE_STYLE_FILL_AREA ( #7799 ) ;
#4503 = CARTESIAN_POINT ( 'NONE',  ( 0.000000000000000000, 216.7545334744432921, 205.1946179577815883 ) ) ;
#4504 = EDGE_CURVE ( 'NONE', #17622, #12429, #12042, .T. ) ;
#4505 = DIRECTION ( 'NONE',  ( -1.000000000000000000, 0.000000000000000000, 7.709882115452498874E-16 ) ) ;
#4506 = AXIS2_PLACEMENT_3D ( 'NONE', #11822, #2424, #6890 ) ;
#4507 = DIRECTION ( 'NONE',  ( 0.7976179040349731242, 0.000000000000000000, 0.6031630618355673379 ) ) ;
#4508 = CARTESIAN_POINT ( 'NONE',  ( 53.48937290013659407, 129.7247684487574588, 283.6050404526570219 ) ) ;
#4509 = FACE_OUTER_BOUND ( 'NONE', #8511, .T. ) ;
#4510 = EDGE_CURVE ( 'NONE', #14656, #2143, #2841, .T. ) ;
#4511 = DIRECTION ( 'NONE',  ( 0.000000000000000000, 0.000000000000000000, 1.000000000000000000 ) ) ;
#4512 = SURFACE_STYLE_FILL_AREA ( #15547 ) ;
#4513 = VERTEX_POINT ( 'NONE', #13869 ) ;
#4514 = EDGE_CURVE ( 'NONE', #17286, #12308, #8926, .T. ) ;
#4515 = VERTEX_POINT ( 'NONE', #7395 ) ;
#4516 = ORIENTED_EDGE ( 'NONE', *, *, #294, .T. ) ;
#4517 = ORIENTED_EDGE ( 'NONE', *, *, #19290, .F. ) ;
#4518 = SURFACE_SIDE_STYLE ('',( #176 ) ) ;
#4519 = CARTESIAN_POINT ( 'NONE',  ( -79.35594118700021227, 138.8781009637241368, 489.5670100215901357 ) ) ;
#4520 = ORIENTED_EDGE ( 'NONE', *, *, #11923, .T. ) ;
#4521 = LINE ( 'NONE', #274, #15976 ) ;
#4522 = LINE ( 'NONE', #9356, #11629 ) ;
#4523 = ORIENTED_EDGE ( 'NONE', *, *, #19935, .F. ) ;
#4524 = FILL_AREA_STYLE_COLOUR ( '', #18392 ) ;
#4525 = DIRECTION ( 'NONE',  ( 0.000000000000000000, -1.632680918566406547E-16, 1.000000000000000000 ) ) ;
#4526 = DIRECTION ( 'NONE',  ( 0.000000000000000000, 0.7642367632649269549, -0.6449357872488920007 ) ) ;
#4527 = CARTESIAN_POINT ( 'NONE',  ( -0.7808854937525574469, 62.90333651941379145, 9.469847369592788056 ) ) ;
#4528 = FILL_AREA_STYLE_COLOUR ( '', #3872 ) ;
#4529 = CARTESIAN_POINT ( 'NONE',  ( -40.00000000000000000, 0.000000000000000000, -25.99999999999999645 ) ) ;
#4530 = CARTESIAN_POINT ( 'NONE',  ( 31.00000000000000000, 19.00000000000000000, 30.99999999999999289 ) ) ;
#4531 = PRESENTATION_STYLE_ASSIGNMENT (( #12753 ) ) ;
#4532 = EDGE_CURVE ( 'NONE', #10206, #12019, #1259, .T. ) ;
#4533 = CARTESIAN_POINT ( 'NONE',  ( -1.000000000000019984, 147.7545334744432921, 496.6642397995874489 ) ) ;
#4534 = DIRECTION ( 'NONE',  ( -0.000000000000000000, -1.000000000000000000, -0.000000000000000000 ) ) ;
#4535 = ORIENTED_EDGE ( 'NONE', *, *, #20322, .F. ) ;
#4536 = ORIENTED_EDGE ( 'NONE', *, *, #13056, .T. ) ;
#4537 = VERTEX_POINT ( 'NONE', #7587 ) ;
#4538 = ORIENTED_EDGE ( 'NONE', *, *, #7689, .F. ) ;
#4539 = ORIENTED_EDGE ( 'NONE', *, *, #16339, .F. ) ;
#4540 = AXIS2_PLACEMENT_3D ( 'NONE', #6437, #17433, #14141 ) ;
#4541 = EDGE_LOOP ( 'NONE', ( #6003, #7380, #10718, #19268 ) ) ;
#4542 = CARTESIAN_POINT ( 'NONE',  ( 78.48937290013662960, 1.675782865040797740E-14, 250.0000000000000000 ) ) ;
#4543 = FILL_AREA_STYLE ('',( #17022 ) ) ;
#4544 = VECTOR ( 'NONE', #11832, 1000.000000000000000 ) ;
#4545 = LINE ( 'NONE', #18243, #4984 ) ;
#4546 = FACE_OUTER_BOUND ( 'NONE', #7410, .T. ) ;
#4547 = ORIENTED_EDGE ( 'NONE', *, *, #6681, .T. ) ;
#4548 = DIRECTION ( 'NONE',  ( 0.000000000000000000, -7.137148015447440312E-15, 1.000000000000000000 ) ) ;
#4549 = SURFACE_SIDE_STYLE ('',( #18850 ) ) ;
#4550 = CARTESIAN_POINT ( 'NONE',  ( 22.99999999999999645, 0.000000000000000000, 31.00000000000006750 ) ) ;
#4551 = SURFACE_STYLE_USAGE ( .BOTH. , #12391 ) ;
#4552 = EDGE_CURVE ( 'NONE', #548, #4581, #16877, .T. ) ;
#4553 = ORIENTED_EDGE ( 'NONE', *, *, #5107, .F. ) ;
#4554 = DIRECTION ( 'NONE',  ( 0.000000000000000000, 0.000000000000000000, -1.000000000000000000 ) ) ;
#4555 = DIRECTION ( 'NONE',  ( 0.000000000000000000, 0.7071067811865336949, -0.7071067811865614505 ) ) ;
#4556 = CARTESIAN_POINT ( 'NONE',  ( 31.00000000000004263, 0.000000000000000000, -25.99999999999999645 ) ) ;
#4557 = VECTOR ( 'NONE', #1992, 1000.000000000000000 ) ;
#4558 = ORIENTED_EDGE ( 'NONE', *, *, #19452, .F. ) ;
#4559 = FACE_BOUND ( 'NONE', #9143, .T. ) ;
#4560 = ORIENTED_EDGE ( 'NONE', *, *, #3244, .F. ) ;
#4561 = EDGE_CURVE ( 'NONE', #18003, #12618, #10885, .T. ) ;
#4562 = DIRECTION ( 'NONE',  ( 0.000000000000000000, 1.000000000000000000, 0.000000000000000000 ) ) ;
#4563 = LINE ( 'NONE', #14241, #2631 ) ;
#4564 = ORIENTED_EDGE ( 'NONE', *, *, #1601, .F. ) ;
#4565 = DIRECTION ( 'NONE',  ( 1.000000000000000000, 0.000000000000000000, -0.000000000000000000 ) ) ;
#4566 = FILL_AREA_STYLE_COLOUR ( '', #5079 ) ;
#4567 = CARTESIAN_POINT ( 'NONE',  ( -78.99999999999995737, 144.4616402556298453, 504.6850550797586834 ) ) ;
#4568 = AXIS2_PLACEMENT_3D ( 'NONE', #13347, #14457, #19483 ) ;
#4569 = CARTESIAN_POINT ( 'NONE',  ( 0.1710018411068576494, 140.8447580977620248, 501.2608735269712383 ) ) ;
#4570 = LINE ( 'NONE', #124, #19978 ) ;
#4571 = CARTESIAN_POINT ( 'NONE',  ( -23.00000000000002132, 0.000000000000000000, 31.00000000000003553 ) ) ;
#4572 = VERTEX_POINT ( 'NONE', #4503 ) ;
#4573 = DIRECTION ( 'NONE',  ( 0.000000000000000000, -0.3129478523439812032, 0.9497703099767279555 ) ) ;
#4574 = PLANE ( 'NONE',  #2981 ) ;
#4575 = PRESENTATION_STYLE_ASSIGNMENT (( #10859 ) ) ;
#4576 = SHAPE_DEFINITION_REPRESENTATION ( #6303, #17354 ) ;
#4577 = ADVANCED_FACE ( 'NONE', ( #20257 ), #12437, .F. ) ;
#4578 = EDGE_LOOP ( 'NONE', ( #7378, #18866, #4237, #11123, #18970, #1786, #15726, #13323 ) ) ;
#4579 = VERTEX_POINT ( 'NONE', #5129 ) ;
#4580 = ORIENTED_EDGE ( 'NONE', *, *, #9385, .F. ) ;
#4581 = VERTEX_POINT ( 'NONE', #3475 ) ;
#4582 = CONICAL_SURFACE ( 'NONE', #14492, 1.800000000000000266, 0.7853981633974524978 ) ;
#4583 = EDGE_CURVE ( 'NONE', #17875, #10467, #19009, .T. ) ;
#4584 = VECTOR ( 'NONE', #6873, 1000.000000000000000 ) ;
#4585 = EDGE_LOOP ( 'NONE', ( #9679, #14488, #17716, #15474 ) ) ;
#4586 = LINE ( 'NONE', #7879, #513 ) ;
#4587 = ORIENTED_EDGE ( 'NONE', *, *, #1002, .F. ) ;
#4588 = CARTESIAN_POINT ( 'NONE',  ( 0.1178092222713691406, 140.9311717929738279, 501.3355664049633447 ) ) ;
#4589 = ADVANCED_FACE ( 'NONE', ( #12752 ), #160, .F. ) ;
#4590 = CARTESIAN_POINT ( 'NONE',  ( 0.000000000000000000, 145.9162550801369491, 0.000000000000000000 ) ) ;
#4591 = CARTESIAN_POINT ( 'NONE',  ( -22.00000000000001776, 8.000000000000000000, 36.00000000000000711 ) ) ;
#4592 = ADVANCED_FACE ( 'NONE', ( #1800 ), #20347, .F. ) ;
#4593 = APPLICATION_CONTEXT ( 'automotive_design' ) ;
#4594 = PRESENTATION_LAYER_ASSIGNMENT (  '', '', ( #13842 ) ) ;
#4595 = DIRECTION ( 'NONE',  ( -1.000000000000000000, -0.000000000000000000, -0.000000000000000000 ) ) ;
#4596 = DIRECTION ( 'NONE',  ( 1.000000000000000000, 0.000000000000000000, 0.000000000000000000 ) ) ;
#4597 = AXIS2_PLACEMENT_3D ( 'NONE', #4951, #19043, #11334 ) ;
#4598 = FILL_AREA_STYLE ('',( #2635 ) ) ;
#4599 = VECTOR ( 'NONE', #19907, 1000.000000000000000 ) ;
#4600 = CARTESIAN_POINT ( 'NONE',  ( 463.8334540492693350, 134.2156642432025251, 250.0000000000000000 ) ) ;
#4601 = ORIENTED_EDGE ( 'NONE', *, *, #12544, .T. ) ;
#4602 = LINE ( 'NONE', #18497, #1554 ) ;
#4603 = CARTESIAN_POINT ( 'NONE',  ( 475.8334540492694487, 214.2156642432025251, 245.0000000000000000 ) ) ;
#4604 = DIRECTION ( 'NONE',  ( 3.295974604355930324E-14, 3.469446951953611033E-15, -1.000000000000000000 ) ) ;
#4605 = LINE ( 'NONE', #4508, #4143 ) ;
#4606 = CARTESIAN_POINT ( 'NONE',  ( -21.00000000000002842, 0.000000000000000000, -37.50000000000000000 ) ) ;
#4607 = EDGE_CURVE ( 'NONE', #645, #9471, #15848, .T. ) ;
#4608 = DIRECTION ( 'NONE',  ( 0.000000000000000000, 1.000000000000000000, 0.000000000000000000 ) ) ;
#4609 = VERTEX_POINT ( 'NONE', #6462 ) ;
#4610 = ORIENTED_EDGE ( 'NONE', *, *, #6494, .T. ) ;
#4611 = EDGE_CURVE ( 'NONE', #7675, #19389, #15092, .T. ) ;
#4612 = VERTEX_POINT ( 'NONE', #10988 ) ;
#4613 = ORIENTED_EDGE ( 'NONE', *, *, #6146, .F. ) ;
#4614 = CARTESIAN_POINT ( 'NONE',  ( 3.500000000000000000, -14.59999999999999964, -1.787984326755135766E-15 ) ) ;
#4615 = SURFACE_STYLE_USAGE ( .BOTH. , #16791 ) ;
#4616 = VERTEX_POINT ( 'NONE', #6259 ) ;
#4617 = EDGE_CURVE ( 'NONE', #1665, #14262, #4814, .T. ) ;
#4618 = DIRECTION ( 'NONE',  ( 0.000000000000000000, 0.000000000000000000, 1.000000000000000000 ) ) ;
#4619 = DIRECTION ( 'NONE',  ( 1.000000000000000000, 0.000000000000000000, 0.000000000000000000 ) ) ;
#4620 = VERTEX_POINT ( 'NONE', #12962 ) ;
#4621 = DIRECTION ( 'NONE',  ( -0.000000000000000000, -1.000000000000000000, 0.000000000000000000 ) ) ;
#4622 = CARTESIAN_POINT ( 'NONE',  ( -0.000000000000000000, 167.9162550801369491, 250.0000000000000000 ) ) ;
#4623 = CARTESIAN_POINT ( 'NONE',  ( 31.00000000000000000, 11.00000000000000000, -31.00000000000000355 ) ) ;
#4624 = CARTESIAN_POINT ( 'NONE',  ( 55.98937290013660117, 131.2883416677198625, 282.8521325859588842 ) ) ;
#4625 = MECHANICAL_DESIGN_GEOMETRIC_PRESENTATION_REPRESENTATION (  '', ( #9218 ), #16799 ) ;
#4626 = FACE_OUTER_BOUND ( 'NONE', #14903, .T. ) ;
#4627 = CARTESIAN_POINT ( 'NONE',  ( -20.99999999999999645, 19.00000000000000000, 31.00000000000003197 ) ) ;
#4628 = CIRCLE ( 'NONE', #3963, 4.999999999999997335 ) ;
#4629 = DIRECTION ( 'NONE',  ( 0.000000000000000000, 1.000000000000000000, 0.000000000000000000 ) ) ;
#4630 = PRESENTATION_LAYER_ASSIGNMENT (  '', '', ( #6289 ) ) ;
#4631 = STYLED_ITEM ( 'NONE', ( #1524 ), #6305 ) ;
#4632 = CARTESIAN_POINT ( 'NONE',  ( -40.00000000000000000, 68.00000000000000000, -25.99999999999999645 ) ) ;
#4633 = LINE ( 'NONE', #17195, #12832 ) ;
#4634 = ADVANCED_FACE ( 'NONE', ( #9335 ), #17161, .T. ) ;
#4635 = ORIENTED_EDGE ( 'NONE', *, *, #20156, .F. ) ;
#4636 = VERTEX_POINT ( 'NONE', #16063 ) ;
#4637 = ORIENTED_EDGE ( 'NONE', *, *, #5992, .F. ) ;
#4638 = EDGE_LOOP ( 'NONE', ( #597, #11996, #15055, #6569, #16859, #10769 ) ) ;
#4639 = ORIENTED_EDGE ( 'NONE', *, *, #18117, .T. ) ;
#4640 = EDGE_CURVE ( 'NONE', #1837, #20367, #12793, .T. ) ;
#4641 = EDGE_LOOP ( 'NONE', ( #9935, #1111, #1811, #19493 ) ) ;
#4642 = DIRECTION ( 'NONE',  ( 0.000000000000000000, 0.000000000000000000, -1.000000000000000000 ) ) ;
#4643 =( GEOMETRIC_REPRESENTATION_CONTEXT ( 3 ) GLOBAL_UNCERTAINTY_ASSIGNED_CONTEXT ( ( #18542 ) ) GLOBAL_UNIT_ASSIGNED_CONTEXT ( ( #9073, #15462, #9161 ) ) REPRESENTATION_CONTEXT ( 'NONE', 'WORKASPACE' ) );
#4644 = MECHANICAL_DESIGN_GEOMETRIC_PRESENTATION_REPRESENTATION (  '', ( #15509 ), #4303 ) ;
#4645 = CARTESIAN_POINT ( 'NONE',  ( 498.8117674897343932, 191.8198460455371333, 24.99421986894476078 ) ) ;
#4646 = CYLINDRICAL_SURFACE ( 'NONE', #8759, 4.999999999999997335 ) ;
#4647 = PRODUCT_DEFINITION_SHAPE ( 'NONE', 'NONE',  #13881 ) ;
#4648 = FILL_AREA_STYLE_COLOUR ( '', #19186 ) ;
#4649 = DIRECTION ( 'NONE',  ( 1.000000000000000000, 0.000000000000000000, 0.000000000000000000 ) ) ;
#4650 = LINE ( 'NONE', #6106, #89 ) ;
#4651 = DIRECTION ( 'NONE',  ( 1.000000000000000000, -0.000000000000000000, -0.000000000000000000 ) ) ;
#4652 = CARTESIAN_POINT ( 'NONE',  ( 458.8334540492693350, 191.8198460455371333, 215.0057801310552179 ) ) ;
#4653 = DIRECTION ( 'NONE',  ( 0.000000000000000000, 7.137148015447440312E-15, -1.000000000000000000 ) ) ;
#4654 = ORIENTED_EDGE ( 'NONE', *, *, #7986, .T. ) ;
#4655 = CARTESIAN_POINT ( 'NONE',  ( 3.850000000000000089, 1.778491767751089605E-15, 14.27500000000000036 ) ) ;
#4656 = VECTOR ( 'NONE', #14414, 1000.000000000000000 ) ;
#4657 = ORIENTED_EDGE ( 'NONE', *, *, #10607, .F. ) ;
#4658 = ADVANCED_FACE ( 'NONE', ( #1893 ), #6562, .T. ) ;
#4659 = CARTESIAN_POINT ( 'NONE',  ( 423.8334540492694487, 191.8198460455371333, 235.0057801310552463 ) ) ;
#4660 = ORIENTED_EDGE ( 'NONE', *, *, #8031, .T. ) ;
#4661 = CARTESIAN_POINT ( 'NONE',  ( 498.8334540492693918, 214.2156642432025251, 250.0000000000000000 ) ) ;
#4662 = VERTEX_POINT ( 'NONE', #5014 ) ;
#4663 = SURFACE_STYLE_FILL_AREA ( #7657 ) ;
#4664 = SURFACE_STYLE_USAGE ( .BOTH. , #7559 ) ;
#4665 = DIRECTION ( 'NONE',  ( -1.000000000000000000, 0.000000000000000000, 5.551115123125782702E-14 ) ) ;
#4666 = AXIS2_PLACEMENT_3D ( 'NONE', #17175, #17383, #11004 ) ;
#4667 = FACE_OUTER_BOUND ( 'NONE', #17355, .T. ) ;
#4668 = LINE ( 'NONE', #10959, #894 ) ;
#4669 = DIRECTION ( 'NONE',  ( -0.000000000000000000, -1.000000000000000000, -0.000000000000000000 ) ) ;
#4670 = SURFACE_STYLE_USAGE ( .BOTH. , #16848 ) ;
#4671 = ORIENTED_EDGE ( 'NONE', *, *, #12305, .T. ) ;
#4672 = DIRECTION ( 'NONE',  ( -1.000000000000000000, -0.000000000000000000, -0.000000000000000000 ) ) ;
#4673 = CARTESIAN_POINT ( 'NONE',  ( -39.99999999999999289, 8.000000000000000000, 34.99999999999997868 ) ) ;
#4674 = FACE_OUTER_BOUND ( 'NONE', #4359, .T. ) ;
#4675 = CARTESIAN_POINT ( 'NONE',  ( -81.18192946989275072, 140.4048636633015406, 499.8237260975782874 ) ) ;
#4676 = VERTEX_POINT ( 'NONE', #10245 ) ;
#4677 = VECTOR ( 'NONE', #135, 1000.000000000000000 ) ;
#4678 = EDGE_LOOP ( 'NONE', ( #13803, #8584, #11165, #5437 ) ) ;
#4679 = COLOUR_RGB ( '', 0.08235294, 0.09019608, 0.10196078) ;
#4680 = VERTEX_POINT ( 'NONE', #5519 ) ;
#4681 = ADVANCED_BREP_SHAPE_REPRESENTATION ( '', ( #1264, #2741 ), #7323 ) ;
#4682 = LINE ( 'NONE', #3343, #16974 ) ;
#4683 =( GEOMETRIC_REPRESENTATION_CONTEXT ( 3 ) GLOBAL_UNCERTAINTY_ASSIGNED_CONTEXT ( ( #19743 ) ) GLOBAL_UNIT_ASSIGNED_CONTEXT ( ( #11620, #9875, #11736 ) ) REPRESENTATION_CONTEXT ( 'NONE', 'WORKASPACE' ) );
#4684 = AXIS2_PLACEMENT_3D ( 'NONE', #4836, #279, #5038 ) ;
#4685 = ORIENTED_EDGE ( 'NONE', *, *, #18355, .F. ) ;
#4686 = DIRECTION ( 'NONE',  ( 0.000000000000000000, -1.000000000000000000, 0.000000000000000000 ) ) ;
#4687 = VERTEX_POINT ( 'NONE', #10150 ) ;
#4688 = EDGE_CURVE ( 'NONE', #17942, #7810, #18067, .T. ) ;
#4689 = CYLINDRICAL_SURFACE ( 'NONE', #7888, 35.00000000000000711 ) ;
#4690 = CIRCLE ( 'NONE', #17838, 1.000000000000000888 ) ;
#4691 = MECHANICAL_DESIGN_GEOMETRIC_PRESENTATION_REPRESENTATION (  '', ( #3720 ), #8968 ) ;
#4692 = PLANE ( 'NONE',  #12355 ) ;
#4693 =( LENGTH_UNIT ( ) NAMED_UNIT ( * ) SI_UNIT ( .MILLI., .METRE. ) );
#4694 = DIRECTION ( 'NONE',  ( 0.000000000000000000, 0.000000000000000000, -1.000000000000000000 ) ) ;
#4695 = EDGE_CURVE ( 'NONE', #15257, #7254, #18367, .T. ) ;
#4696 = AXIS2_PLACEMENT_3D ( 'NONE', #4591, #3155, #9435 ) ;
#4697 = EDGE_LOOP ( 'NONE', ( #7228, #4928, #14993, #2776 ) ) ;
#4698 = DIRECTION ( 'NONE',  ( 0.000000000000000000, 0.000000000000000000, -1.000000000000000000 ) ) ;
#4699 = CARTESIAN_POINT ( 'NONE',  ( 0.000000000000000000, 372.8685141053783241, -146.8198051533979935 ) ) ;
#4700 = LINE ( 'NONE', #1485, #2402 ) ;
#4701 = PLANE ( 'NONE',  #14961 ) ;
#4702 = CARTESIAN_POINT ( 'NONE',  ( -1.170604780609792455E-14, 142.0976792249509231, 502.3210940490797611 ) ) ;
#4703 = ORIENTED_EDGE ( 'NONE', *, *, #12904, .T. ) ;
#4704 = PRESENTATION_LAYER_ASSIGNMENT (  '', '', ( #8980 ) ) ;
#4705 = DIRECTION ( 'NONE',  ( 0.000000000000000000, -0.6381222063396385646, 0.7699350945217602327 ) ) ;
#4706 = DIRECTION ( 'NONE',  ( 0.000000000000000000, 0.000000000000000000, -1.000000000000000000 ) ) ;
#4707 = VERTEX_POINT ( 'NONE', #754 ) ;
#4708 = ORIENTED_EDGE ( 'NONE', *, *, #8936, .F. ) ;
#4709 = EDGE_CURVE ( 'NONE', #664, #8243, #6968, .T. ) ;
#4710 = AXIS2_PLACEMENT_3D ( 'NONE', #724, #14449, #19382 ) ;
#4711 = AXIS2_PLACEMENT_3D ( 'NONE', #18963, #11136, #7751 ) ;
#4712 = ORIENTED_EDGE ( 'NONE', *, *, #8240, .F. ) ;
#4713 = FACE_OUTER_BOUND ( 'NONE', #19789, .T. ) ;
#4714 = CARTESIAN_POINT ( 'NONE',  ( -79.03568289232478605, 140.4747598996043507, 501.9652730068947335 ) ) ;
#4715 = ORIENTED_EDGE ( 'NONE', *, *, #17733, .F. ) ;
#4716 = DIRECTION ( 'NONE',  ( 1.000000000000000000, 0.000000000000000000, 0.000000000000000000 ) ) ;
#4717 = ADVANCED_FACE ( 'NONE', ( #17981 ), #3874, .T. ) ;
#4718 = CARTESIAN_POINT ( 'NONE',  ( -25.99999999999999645, 68.00000000000000000, -39.99999999999999289 ) ) ;
#4719 = CLOSED_SHELL ( 'NONE', ( #17786, #12124, #7362, #16227, #14509, #14853, #11393, #6214, #16193, #10903, #18929, #11917, #18911, #1321, #9624, #14169, #6993, #14002, #5022, #192, #7251, #343, #20192, #3321, #19322, #7501 ) ) ;
#4720 = AXIS2_PLACEMENT_3D ( 'NONE', #19136, #11018, #12561 ) ;
#4721 = ORIENTED_EDGE ( 'NONE', *, *, #20310, .F. ) ;
#4722 = FACE_BOUND ( 'NONE', #4357, .T. ) ;
#4723 = DIRECTION ( 'NONE',  ( -1.000000000000000000, -1.595148023886719315E-16, 0.000000000000000000 ) ) ;
#4724 = CARTESIAN_POINT ( 'NONE',  ( -1.734723475976807094E-15, 60.00000000000000711, 6.000000000000000000 ) ) ;
#4725 = CARTESIAN_POINT ( 'NONE',  ( 40.00000000000001421, 0.000000000000000000, 0.000000000000000000 ) ) ;
#4726 = EDGE_CURVE ( 'NONE', #5319, #6868, #14425, .T. ) ;
#4727 = DIRECTION ( 'NONE',  ( 0.000000000000000000, -1.000000000000000000, 0.000000000000000000 ) ) ;
#4728 = AXIS2_PLACEMENT_3D ( 'NONE', #19360, #4596, #13979 ) ;
#4729 = PRESENTATION_LAYER_ASSIGNMENT (  '', '', ( #4066 ) ) ;
#4730 = DIRECTION ( 'NONE',  ( 0.000000000000000000, 0.000000000000000000, -1.000000000000000000 ) ) ;
#4731 = SURFACE_SIDE_STYLE ('',( #15460 ) ) ;
#4732 = VECTOR ( 'NONE', #9060, 1000.000000000000000 ) ;
#4733 = EDGE_CURVE ( 'NONE', #13911, #6449, #11808, .T. ) ;
#4734 = DIRECTION ( 'NONE',  ( 1.016981637791458695E-13, 0.000000000000000000, 1.000000000000000000 ) ) ;
#4735 = CARTESIAN_POINT ( 'NONE',  ( 0.000000000000000000, 0.000000000000000000, 250.0000000000000000 ) ) ;
#4736 = ADVANCED_FACE ( 'NONE', ( #5423, #19319 ), #16263, .F. ) ;
#4737 = AXIS2_PLACEMENT_3D ( 'NONE', #14164, #252, #10875 ) ;
#4738 = DIRECTION ( 'NONE',  ( -0.000000000000000000, -1.000000000000000000, -0.000000000000000000 ) ) ;
#4739 = AXIS2_PLACEMENT_3D ( 'NONE', #1610, #12680, #83 ) ;
#4740 = EDGE_CURVE ( 'NONE', #12937, #17794, #6213, .T. ) ;
#4741 = VERTEX_POINT ( 'NONE', #14887 ) ;
#4742 = PRESENTATION_LAYER_ASSIGNMENT (  '', '', ( #14626 ) ) ;
#4743 = ORIENTED_EDGE ( 'NONE', *, *, #19777, .T. ) ;
#4744 = CARTESIAN_POINT ( 'NONE',  ( 22.99999999999999289, 68.00000000000000000, 37.00000000000002132 ) ) ;
#4745 = EDGE_LOOP ( 'NONE', ( #10570, #528, #17907, #4488 ) ) ;
#4746 = ORIENTED_EDGE ( 'NONE', *, *, #220, .F. ) ;
#4747 = STYLED_ITEM ( 'NONE', ( #12877 ), #12371 ) ;
#4748 = AXIS2_PLACEMENT_3D ( 'NONE', #5402, #5502, #17756 ) ;
#4749 = ORIENTED_EDGE ( 'NONE', *, *, #8429, .F. ) ;
#4750 = DIRECTION ( 'NONE',  ( 0.000000000000000000, 0.000000000000000000, 1.000000000000000000 ) ) ;
#4751 = VECTOR ( 'NONE', #2710, 1000.000000000000000 ) ;
#4752 = ORIENTED_EDGE ( 'NONE', *, *, #1144, .T. ) ;
#4753 =( NAMED_UNIT ( * ) SI_UNIT ( $, .STERADIAN. ) SOLID_ANGLE_UNIT ( ) );
#4754 = DIRECTION ( 'NONE',  ( 0.000000000000000000, 0.000000000000000000, -1.000000000000000000 ) ) ;
#4755 = FACE_OUTER_BOUND ( 'NONE', #4454, .T. ) ;
#4756 = DIRECTION ( 'NONE',  ( 0.000000000000000000, -1.000000000000000000, 0.000000000000000000 ) ) ;
#4757 = MECHANICAL_DESIGN_GEOMETRIC_PRESENTATION_REPRESENTATION (  '', ( #11000 ), #12655 ) ;
#4758 = CARTESIAN_POINT ( 'NONE',  ( 82.88953019741013861, 80.91625508013694912, 250.0000000000000000 ) ) ;
#4759 = AXIS2_PLACEMENT_3D ( 'NONE', #5866, #7514, #10702 ) ;
#4760 = DIRECTION ( 'NONE',  ( -0.000000000000000000, -0.000000000000000000, 1.000000000000000000 ) ) ;
#4761 =( GEOMETRIC_REPRESENTATION_CONTEXT ( 3 ) GLOBAL_UNCERTAINTY_ASSIGNED_CONTEXT ( ( #749 ) ) GLOBAL_UNIT_ASSIGNED_CONTEXT ( ( #9296, #15910, #6430 ) ) REPRESENTATION_CONTEXT ( 'NONE', 'WORKASPACE' ) );
#4762 = FACE_OUTER_BOUND ( 'NONE', #19992, .T. ) ;
#4763 = FACE_OUTER_BOUND ( 'NONE', #5183, .T. ) ;
#4764 = ORIENTED_EDGE ( 'NONE', *, *, #13776, .F. ) ;
#4765 = DIRECTION ( 'NONE',  ( 1.000000000000000000, 0.000000000000000000, 0.000000000000000000 ) ) ;
#4766 = EDGE_CURVE ( 'NONE', #688, #7437, #14099, .T. ) ;
#4767 = VECTOR ( 'NONE', #14917, 1000.000000000000000 ) ;
#4768 = MECHANICAL_DESIGN_GEOMETRIC_PRESENTATION_REPRESENTATION (  '', ( #2773 ), #19240 ) ;
#4769 = PRESENTATION_LAYER_ASSIGNMENT (  '', '', ( #8702 ) ) ;
#4770 = PRESENTATION_LAYER_ASSIGNMENT (  '', '', ( #6756 ) ) ;
#4771 = EDGE_CURVE ( 'NONE', #19489, #15985, #16755, .T. ) ;
#4772 = ADVANCED_FACE ( 'NONE', ( #8714 ), #7074, .T. ) ;
#4773 = VECTOR ( 'NONE', #20183, 1000.000000000000000 ) ;
#4774 =( GEOMETRIC_REPRESENTATION_CONTEXT ( 3 ) GLOBAL_UNCERTAINTY_ASSIGNED_CONTEXT ( ( #2286 ) ) GLOBAL_UNIT_ASSIGNED_CONTEXT ( ( #1502, #1385, #7816 ) ) REPRESENTATION_CONTEXT ( 'NONE', 'WORKASPACE' ) );
#4775 = ORIENTED_EDGE ( 'NONE', *, *, #18807, .T. ) ;
#4776 = CARTESIAN_POINT ( 'NONE',  ( -211.5106270998635409, 113.1299228374912502, 220.6387154965113382 ) ) ;
#4777 = ORIENTED_EDGE ( 'NONE', *, *, #18946, .F. ) ;
#4778 = TOROIDAL_SURFACE ( 'NONE', #13982, 8.000000000000000000, 1.000000000000000000 ) ;
#4779 = ORIENTED_EDGE ( 'NONE', *, *, #15467, .T. ) ;
#4780 = DIRECTION ( 'NONE',  ( 0.000000000000000000, 0.000000000000000000, -1.000000000000000000 ) ) ;
#4781 = CIRCLE ( 'NONE', #7421, 3.883636366625808911 ) ;
#4782 = DIRECTION ( 'NONE',  ( 1.000000000000000000, 0.000000000000000000, 0.000000000000000000 ) ) ;
#4783 = CARTESIAN_POINT ( 'NONE',  ( 0.6480199899356283710, 140.4585494651481099, 500.8850776723155036 ) ) ;
#4784 = CARTESIAN_POINT ( 'NONE',  ( 0.000000000000000000, -5.000000000000000888, -150.0000000000000000 ) ) ;
#4785 = CIRCLE ( 'NONE', #14985, 4.999999999999990230 ) ;
#4786 = CARTESIAN_POINT ( 'NONE',  ( 36.99999999999999289, 10.00000000000000000, -22.99999999999999645 ) ) ;
#4787 = FILL_AREA_STYLE_COLOUR ( '', #4121 ) ;
#4788 = VECTOR ( 'NONE', #15532, 1000.000000000000000 ) ;
#4789 = ORIENTED_EDGE ( 'NONE', *, *, #18288, .T. ) ;
#4790 = DIRECTION ( 'NONE',  ( 0.000000000000000000, 1.000000000000000000, 0.000000000000000000 ) ) ;
#4791 = DIRECTION ( 'NONE',  ( -0.000000000000000000, 0.000000000000000000, 1.000000000000000000 ) ) ;
#4792 = PRESENTATION_STYLE_ASSIGNMENT (( #12611 ) ) ;
#4793 = EDGE_CURVE ( 'NONE', #14489, #12201, #14697, .T. ) ;
#4794 = ORIENTED_EDGE ( 'NONE', *, *, #11378, .F. ) ;
#4795 = ORIENTED_EDGE ( 'NONE', *, *, #18429, .F. ) ;
#4796 = FILL_AREA_STYLE ('',( #1342 ) ) ;
#4797 = ORIENTED_EDGE ( 'NONE', *, *, #15255, .F. ) ;
#4798 = ORIENTED_EDGE ( 'NONE', *, *, #13797, .T. ) ;
#4799 = COLOUR_RGB ( '', 0.31764706, 0.68627451, 0.89019608) ;
#4800 = ORIENTED_EDGE ( 'NONE', *, *, #1036, .F. ) ;
#4801 = STYLED_ITEM ( 'NONE', ( #13435 ), #2347 ) ;
#4802 = FACE_OUTER_BOUND ( 'NONE', #3921, .T. ) ;
#4803 = ORIENTED_EDGE ( 'NONE', *, *, #4853, .F. ) ;
#4804 = CARTESIAN_POINT ( 'NONE',  ( 458.8334540492693350, 191.8198460455371333, 81.76606011801540319 ) ) ;
#4805 = PLANE ( 'NONE',  #16174 ) ;
#4806 = CONICAL_SURFACE ( 'NONE', #17300, 12.64907335584850046, 0.003530080289784348537 ) ;
#4807 = ORIENTED_EDGE ( 'NONE', *, *, #10295, .T. ) ;
#4808 = DIRECTION ( 'NONE',  ( 1.000000000000000000, 0.000000000000000000, -0.000000000000000000 ) ) ;
#4809 = DIRECTION ( 'NONE',  ( 0.000000000000000000, 0.000000000000000000, -1.000000000000000000 ) ) ;
#4810 = DIRECTION ( 'NONE',  ( 1.000000000000000000, 0.000000000000000000, 0.000000000000000000 ) ) ;
#4811 = SURFACE_SIDE_STYLE ('',( #12531 ) ) ;
#4812 = SURFACE_STYLE_USAGE ( .BOTH. , #12532 ) ;
#4813 = ORIENTED_EDGE ( 'NONE', *, *, #12566, .T. ) ;
#4814 = LINE ( 'NONE', #12642, #16417 ) ;
#4815 = LINE ( 'NONE', #20258, #9610 ) ;
#4816 = DIRECTION ( 'NONE',  ( -1.000000000000000000, -1.694044051971171780E-15, -1.283989322801278906E-15 ) ) ;
#4817 = SHAPE_REPRESENTATION_RELATIONSHIP ( 'NONE' , 'NONE' ,  #6180, #1492 ) ;
#4818 = CARTESIAN_POINT ( 'NONE',  ( -39.99999999999999289, 0.000000000000000000, -34.99999999999997868 ) ) ;
#4819 = CARTESIAN_POINT ( 'NONE',  ( 35.00000000000000711, 19.00000000000000000, -21.00000000000000355 ) ) ;
#4820 = CIRCLE ( 'NONE', #11385, 8.000000000000007105 ) ;
#4821 = ORIENTED_EDGE ( 'NONE', *, *, #6278, .F. ) ;
#4822 = AXIS2_PLACEMENT_3D ( 'NONE', #2980, #4642, #1521 ) ;
#4823 = ORIENTED_EDGE ( 'NONE', *, *, #2740, .F. ) ;
#4824 = PRODUCT ( 'TAS-006', 'TAS-006', '', ( #1143 ) ) ;
#4825 = EDGE_CURVE ( 'NONE', #13802, #2872, #3579, .T. ) ;
#4826 = ORIENTED_EDGE ( 'NONE', *, *, #3781, .T. ) ;
#4827 = CARTESIAN_POINT ( 'NONE',  ( 1.399999999999999911, -15.25000000000000000, -1.867586368699713770E-15 ) ) ;
#4828 = CARTESIAN_POINT ( 'NONE',  ( -79.91604175977239777, 139.6462705220292548, 500.5714951779720536 ) ) ;
#4829 = ORIENTED_EDGE ( 'NONE', *, *, #7116, .F. ) ;
#4830 = AXIS2_PLACEMENT_3D ( 'NONE', #7518, #986, #7610 ) ;
#4831 = SURFACE_STYLE_USAGE ( .BOTH. , #15668 ) ;
#4832 = ORIENTED_EDGE ( 'NONE', *, *, #14792, .F. ) ;
#4833 = ADVANCED_FACE ( 'NONE', ( #9951 ), #13159, .F. ) ;
#4834 = DIRECTION ( 'NONE',  ( 0.000000000000000000, 1.000000000000000000, 0.000000000000000000 ) ) ;
#4835 = MECHANICAL_DESIGN_GEOMETRIC_PRESENTATION_REPRESENTATION (  '', ( #4179 ), #1843 ) ;
#4836 = CARTESIAN_POINT ( 'NONE',  ( 55.48937290013660117, 127.7247684487574304, 368.0000000000000000 ) ) ;
#4837 =( NAMED_UNIT ( * ) PLANE_ANGLE_UNIT ( ) SI_UNIT ( $, .RADIAN. ) );
#4838 = CARTESIAN_POINT ( 'NONE',  ( -1.512611822017144947, 62.62004896476273785, 9.385845453595075938 ) ) ;
#4839 = FACE_BOUND ( 'NONE', #10586, .T. ) ;
#4840 = CARTESIAN_POINT ( 'NONE',  ( -78.99999999999995737, 152.4824555358010798, 501.3921618609452366 ) ) ;
#4841 = CARTESIAN_POINT ( 'NONE',  ( -31.00000000000000000, 19.00000000000000000, 30.99999999999999289 ) ) ;
#4842 = CARTESIAN_POINT ( 'NONE',  ( -25.99999999999999645, 68.00000000000000000, -39.99999999999999289 ) ) ;
#4843 =( LENGTH_UNIT ( ) NAMED_UNIT ( * ) SI_UNIT ( .MILLI., .METRE. ) );
#4844 = SURFACE_STYLE_USAGE ( .BOTH. , #10813 ) ;
#4845 = EDGE_CURVE ( 'NONE', #19815, #18235, #18380, .T. ) ;
#4846 = ORIENTED_EDGE ( 'NONE', *, *, #16216, .F. ) ;
#4847 = ORIENTED_EDGE ( 'NONE', *, *, #14530, .T. ) ;
#4848 = ADVANCED_FACE ( 'NONE', ( #19806 ), #4185, .T. ) ;
#4849 = ORIENTED_EDGE ( 'NONE', *, *, #3308, .T. ) ;
#4850 = ORIENTED_EDGE ( 'NONE', *, *, #15326, .T. ) ;
#4851 = VERTEX_POINT ( 'NONE', #5712 ) ;
#4852 = DIRECTION ( 'NONE',  ( 1.000000000000000000, 0.000000000000000000, 0.000000000000000000 ) ) ;
#4853 = EDGE_CURVE ( 'NONE', #9760, #7832, #612, .T. ) ;
#4854 = DIRECTION ( 'NONE',  ( 0.000000000000000000, 0.000000000000000000, -1.000000000000000000 ) ) ;
#4855 = DIRECTION ( 'NONE',  ( 0.000000000000000000, 0.000000000000000000, 1.000000000000000000 ) ) ;
#4856 = ADVANCED_FACE ( 'NONE', ( #2613 ), #4073, .T. ) ;
#4857 = FILL_AREA_STYLE_COLOUR ( '', #12866 ) ;
#4858 = ADVANCED_FACE ( 'NONE', ( #1335 ), #16666, .F. ) ;
#4859 = PLANE ( 'NONE',  #18291 ) ;
#4860 = VERTEX_POINT ( 'NONE', #5828 ) ;
#4861 = DIRECTION ( 'NONE',  ( 1.000000000000000000, -0.000000000000000000, 0.000000000000000000 ) ) ;
#4862 = AXIS2_PLACEMENT_3D ( 'NONE', #10193, #19562, #3826 ) ;
#4863 = DIRECTION ( 'NONE',  ( -0.000000000000000000, -1.000000000000000000, -0.000000000000000000 ) ) ;
#4864 = CARTESIAN_POINT ( 'NONE',  ( 0.000000000000000000, 216.7545334744432921, 515.1946179577817020 ) ) ;
#4865 = DIRECTION ( 'NONE',  ( 1.000000000000000000, 0.000000000000000000, 0.000000000000000000 ) ) ;
#4866 = DIRECTION ( 'NONE',  ( 0.000000000000000000, 1.000000000000000000, 0.000000000000000000 ) ) ;
#4867 = ORIENTED_EDGE ( 'NONE', *, *, #14743, .T. ) ;
#4868 = ADVANCED_FACE ( 'NONE', ( #12105 ), #1234, .F. ) ;
#4869 = AXIS2_PLACEMENT_3D ( 'NONE', #10082, #16287, #8443 ) ;
#4870 = ORIENTED_EDGE ( 'NONE', *, *, #15566, .F. ) ;
#4871 = ADVANCED_FACE ( 'NONE', ( #12298 ), #2816, .F. ) ;
#4872 = CARTESIAN_POINT ( 'NONE',  ( -39.99999999999999289, 0.000000000000000000, 34.99999999999997868 ) ) ;
#4873 = ORIENTED_EDGE ( 'NONE', *, *, #2608, .F. ) ;
#4874 = PRESENTATION_STYLE_ASSIGNMENT (( #8070 ) ) ;
#4875 = ORIENTED_EDGE ( 'NONE', *, *, #910, .T. ) ;
#4876 = CARTESIAN_POINT ( 'NONE',  ( 10.00000000000000000, 5.352861011586007481E-13, -75.00000000000599698 ) ) ;
#4877 = DIRECTION ( 'NONE',  ( 0.000000000000000000, 1.000000000000000000, 0.000000000000000000 ) ) ;
#4878 = CARTESIAN_POINT ( 'NONE',  ( 0.1064033129882337864, 140.9773519603829754, 501.3703764260786215 ) ) ;
#4879 = CARTESIAN_POINT ( 'NONE',  ( 21.99999999999998224, 10.00000000000000000, -32.99999999999999289 ) ) ;
#4880 = DIRECTION ( 'NONE',  ( 1.000000000000000000, 0.000000000000000000, 0.000000000000000000 ) ) ;
#4881 = VECTOR ( 'NONE', #4698, 1000.000000000000000 ) ;
#4882 = ORIENTED_EDGE ( 'NONE', *, *, #476, .T. ) ;
#4883 = PLANE ( 'NONE',  #12805 ) ;
#4884 = DIRECTION ( 'NONE',  ( -0.000000000000000000, -0.000000000000000000, 1.000000000000000000 ) ) ;
#4885 = PLANE ( 'NONE',  #16607 ) ;
#4886 = SHAPE_DEFINITION_REPRESENTATION ( #9420, #8923 ) ;
#4887 = LINE ( 'NONE', #3019, #6989 ) ;
#4888 = VERTEX_POINT ( 'NONE', #15514 ) ;
#4889 = ORIENTED_EDGE ( 'NONE', *, *, #1180, .F. ) ;
#4890 = EDGE_CURVE ( 'NONE', #10259, #13735, #14760, .T. ) ;
#4891 = ORIENTED_EDGE ( 'NONE', *, *, #7607, .F. ) ;
#4892 = CARTESIAN_POINT ( 'NONE',  ( 40.00000000000000711, 8.000000000000000000, 34.99999999999997868 ) ) ;
#4893 = AXIS2_PLACEMENT_3D ( 'NONE', #6023, #19915, #4366 ) ;
#4894 = VERTEX_POINT ( 'NONE', #15923 ) ;
#4895 = LINE ( 'NONE', #11389, #16620 ) ;
#4896 = B_SPLINE_CURVE_WITH_KNOTS ( 'NONE', 3,
 ( #10097, #2235, #14937, #14823, #20269, #5769, #4519, #15350, #13697, #5864, #6178, #4409, #18720, #12061, #18630, #3055 ),
 .UNSPECIFIED., .F., .F.,
 ( 4, 2, 2, 2, 2, 2, 2, 4 ),
 ( 0.000000000000000000, 0.0004237645333845638696, 0.0008475290667691277391, 0.001695058133538260032, 0.002118822666922774624, 0.002542587200307289651, 0.002966351733691804677, 0.003390116267076319703 ),
 .UNSPECIFIED. ) ;
#4897 = CARTESIAN_POINT ( 'NONE',  ( 98.48937290013662960, 113.1299228374914350, 220.6387154965113382 ) ) ;
#4898 = ORIENTED_EDGE ( 'NONE', *, *, #3605, .T. ) ;
#4899 = CYLINDRICAL_SURFACE ( 'NONE', #15605, 5.000000000000000888 ) ;
#4900 = FILL_AREA_STYLE ('',( #17364 ) ) ;
#4901 = PLANE ( 'NONE',  #7907 ) ;
#4902 = LINE ( 'NONE', #17565, #4046 ) ;
#4903 =( NAMED_UNIT ( * ) PLANE_ANGLE_UNIT ( ) SI_UNIT ( $, .RADIAN. ) );
#4904 = CARTESIAN_POINT ( 'NONE',  ( -0.1969510947806061563, 38.00000000000000711, 9.500000000000003553 ) ) ;
#4905 = EDGE_LOOP ( 'NONE', ( #4005, #13513, #9209, #14772 ) ) ;
#4906 = CARTESIAN_POINT ( 'NONE',  ( 98.48937290013662960, 113.1299228374914350, 170.4174721992565082 ) ) ;
#4907 = DIRECTION ( 'NONE',  ( 0.000000000000000000, 0.000000000000000000, -1.000000000000000000 ) ) ;
#4908 = LINE ( 'NONE', #18802, #19514 ) ;
#4909 = SHAPE_REPRESENTATION_RELATIONSHIP ( 'NONE' , 'NONE' ,  #16721, #15281 ) ;
#4910 = CARTESIAN_POINT ( 'NONE',  ( -211.5106270998635409, 103.1299228374912360, 79.58252780074349175 ) ) ;
#4911 = DIRECTION ( 'NONE',  ( 1.000000000000000000, 0.000000000000000000, 0.000000000000000000 ) ) ;
#4912 = CIRCLE ( 'NONE', #13164, 10.00000000000000888 ) ;
#4913 = CARTESIAN_POINT ( 'NONE',  ( 0.7149011648340997116, 138.7723821175181911, 490.5025619656413483 ) ) ;
#4914 = PRESENTATION_LAYER_ASSIGNMENT (  '', '', ( #18725 ) ) ;
#4915 = FILL_AREA_STYLE ('',( #12540 ) ) ;
#4916 = ORIENTED_EDGE ( 'NONE', *, *, #5231, .T. ) ;
#4917 = CARTESIAN_POINT ( 'NONE',  ( -22.99999999999999645, 68.00000000000000000, 31.00000000000003908 ) ) ;
#4918 = VERTEX_POINT ( 'NONE', #9309 ) ;
#4919 = CARTESIAN_POINT ( 'NONE',  ( 0.000000000000000000, 0.000000000000000000, -150.0000000000000000 ) ) ;
#4920 = CARTESIAN_POINT ( 'NONE',  ( -80.42483422545421945, 139.5159773110449350, 500.2902022611505117 ) ) ;
#4921 = ORIENTED_EDGE ( 'NONE', *, *, #4263, .F. ) ;
#4922 = STYLED_ITEM ( 'NONE', ( #10706 ), #6592 ) ;
#4923 = DIRECTION ( 'NONE',  ( 1.000000000000000000, 5.889072920838430686E-16, -0.000000000000000000 ) ) ;
#4924 = ADVANCED_FACE ( 'NONE', ( #18879 ), #19081, .F. ) ;
#4925 = MECHANICAL_DESIGN_GEOMETRIC_PRESENTATION_REPRESENTATION (  '', ( #8534 ), #18072 ) ;
#4926 = SURFACE_STYLE_FILL_AREA ( #18928 ) ;
#4927 = MECHANICAL_DESIGN_GEOMETRIC_PRESENTATION_REPRESENTATION (  '', ( #8066 ), #11847 ) ;
#4928 = ORIENTED_EDGE ( 'NONE', *, *, #12809, .T. ) ;
#4929 = CARTESIAN_POINT ( 'NONE',  ( 21.99999999999998224, 6.000000000000000000, -35.99999999999999289 ) ) ;
#4930 = DIRECTION ( 'NONE',  ( 0.000000000000000000, 0.000000000000000000, 1.000000000000000000 ) ) ;
#4931 = FACE_BOUND ( 'NONE', #2958, .T. ) ;
#4932 = SURFACE_STYLE_FILL_AREA ( #13281 ) ;
#4933 = FACE_BOUND ( 'NONE', #17937, .T. ) ;
#4934 =( LENGTH_UNIT ( ) NAMED_UNIT ( * ) SI_UNIT ( .MILLI., .METRE. ) );
#4935 = LINE ( 'NONE', #18351, #7331 ) ;
#4936 = CARTESIAN_POINT ( 'NONE',  ( 26.00000000000000000, 19.00000000000000000, 40.00000000000001421 ) ) ;
#4937 = FACE_OUTER_BOUND ( 'NONE', #17666, .T. ) ;
#4938 = LINE ( 'NONE', #6291, #9516 ) ;
#4939 = EDGE_LOOP ( 'NONE', ( #11663, #5023, #14110, #18715 ) ) ;
#4940 = MECHANICAL_DESIGN_GEOMETRIC_PRESENTATION_REPRESENTATION (  '', ( #3631 ), #1270 ) ;
#4941 = AXIS2_PLACEMENT_3D ( 'NONE', #3590, #9553, #5149 ) ;
#4942 = ADVANCED_FACE ( 'NONE', ( #14059 ), #10157, .F. ) ;
#4943 = EDGE_LOOP ( 'NONE', ( #19931, #6912, #7374, #5458, #6942, #9013 ) ) ;
#4944 = ORIENTED_EDGE ( 'NONE', *, *, #19600, .T. ) ;
#4945 = CARTESIAN_POINT ( 'NONE',  ( 0.000000000000000000, 0.000000000000000000, 0.000000000000000000 ) ) ;
#4946 = ORIENTED_EDGE ( 'NONE', *, *, #4263, .T. ) ;
#4947 = EDGE_LOOP ( 'NONE', ( #13959, #18297, #7413, #16832 ) ) ;
#4948 = EDGE_LOOP ( 'NONE', ( #5406, #17429, #5904, #2547 ) ) ;
#4949 = DIRECTION ( 'NONE',  ( 0.000000000000000000, -1.000000000000000000, 0.000000000000000000 ) ) ;
#4950 = LINE ( 'NONE', #17210, #7056 ) ;
#4951 = CARTESIAN_POINT ( 'NONE',  ( 0.000000000000000000, 10.00000000000000000, 0.000000000000000000 ) ) ;
#4952 = AXIS2_PLACEMENT_3D ( 'NONE', #3282, #15875, #4979 ) ;
#4953 = CARTESIAN_POINT ( 'NONE',  ( 25.99999999999997868, 10.00000000000000000, 40.00000000000000711 ) ) ;
#4954 = AXIS2_PLACEMENT_3D ( 'NONE', #16707, #17920, #13205 ) ;
#4955 = VECTOR ( 'NONE', #14142, 1000.000000000000000 ) ;
#4957 = EDGE_CURVE ( 'NONE', #12424, #19242, #1768, .T. ) ;
#4956 = DIRECTION ( 'NONE',  ( 1.000000000000000000, -0.000000000000000000, 0.000000000000000000 ) ) ;
#4958 = DIRECTION ( 'NONE',  ( -8.188278247072579902E-16, 0.7817866094812263578, 0.6235460666509320404 ) ) ;
#4959 = CARTESIAN_POINT ( 'NONE',  ( 0.000000000000000000, 152.4824555358010798, 510.3921618609452935 ) ) ;
#4960 = CARTESIAN_POINT ( 'NONE',  ( 37.00000000000000000, 68.00000000000000000, 23.00000000000001066 ) ) ;
#4961 = ADVANCED_FACE ( 'NONE', ( #17348, #8083 ), #9417, .T. ) ;
#4962 = ORIENTED_EDGE ( 'NONE', *, *, #5893, .T. ) ;
#4963 = DIRECTION ( 'NONE',  ( 1.000000000000000000, -0.000000000000000000, 0.000000000000000000 ) ) ;
#4964 = DIRECTION ( 'NONE',  ( 0.000000000000000000, 0.000000000000000000, -1.000000000000000000 ) ) ;
#4965 = VECTOR ( 'NONE', #755, 1000.000000000000000 ) ;
#4966 = AXIS2_PLACEMENT_3D ( 'NONE', #6740, #18764, #17 ) ;
#4967 = VERTEX_POINT ( 'NONE', #129 ) ;
#4968 = VECTOR ( 'NONE', #12565, 1000.000000000000000 ) ;
#4969 = CARTESIAN_POINT ( 'NONE',  ( 503.8334540492693918, 0.000000000000000000, 0.000000000000000000 ) ) ;
#4970 = ORIENTED_EDGE ( 'NONE', *, *, #14015, .T. ) ;
#4971 = EDGE_CURVE ( 'NONE', #10340, #5163, #15816, .T. ) ;
#4972 = DIRECTION ( 'NONE',  ( 1.000000000000000000, -0.000000000000000000, -0.000000000000000000 ) ) ;
#4973 = VECTOR ( 'NONE', #7523, 1000.000000000000000 ) ;
#4974 = VERTEX_POINT ( 'NONE', #6138 ) ;
#4975 = SURFACE_STYLE_USAGE ( .BOTH. , #1447 ) ;
#4976 = CARTESIAN_POINT ( 'NONE',  ( -20.99999999999999645, 8.000000000000000000, -35.00000000000000711 ) ) ;
#4977 = VERTEX_POINT ( 'NONE', #15727 ) ;
#4978 = LINE ( 'NONE', #3844, #2426 ) ;
#4980 = EDGE_CURVE ( 'NONE', #6211, #2287, #1654, .T. ) ;
#4979 = DIRECTION ( 'NONE',  ( 0.000000000000000000, -7.137148015447440312E-15, 1.000000000000000000 ) ) ;
#4981 = STYLED_ITEM ( 'NONE', ( #4531 ), #11917 ) ;
#4982 = PRESENTATION_LAYER_ASSIGNMENT (  '', '', ( #2671 ) ) ;
#4983 = CARTESIAN_POINT ( 'NONE',  ( 0.3482790861934039195, 140.6280840731730848, 501.0621025226475922 ) ) ;
#4984 = VECTOR ( 'NONE', #11974, 1000.000000000000000 ) ;
#4985 = CARTESIAN_POINT ( 'NONE',  ( 178.4893729001365728, 113.1299228374914918, 170.4174721992565082 ) ) ;
#4986 = CARTESIAN_POINT ( 'NONE',  ( -79.99999999999995737, 216.7545334744432921, 509.3921618609452935 ) ) ;
#4987 = EDGE_LOOP ( 'NONE', ( #8371, #4613, #7623, #3239 ) ) ;
#4988 = DIRECTION ( 'NONE',  ( -0.000000000000000000, -0.000000000000000000, 1.000000000000000000 ) ) ;
#4989 = CARTESIAN_POINT ( 'NONE',  ( 22.99999999999997513, 10.00000000000000000, 31.00000000000005684 ) ) ;
#4990 = DIRECTION ( 'NONE',  ( 0.000000000000000000, 0.000000000000000000, 1.000000000000000000 ) ) ;
#4991 = ADVANCED_FACE ( 'NONE', ( #10963 ), #4883, .F. ) ;
#4992 = PRODUCT_DEFINITION_SHAPE ( 'NONE', 'NONE',  #20374 ) ;
#4993 = CARTESIAN_POINT ( 'NONE',  ( 0.000000000000000000, -3.000000000000000000, 35.00000000000000711 ) ) ;
#4994 = VERTEX_POINT ( 'NONE', #9727 ) ;
#4995 = EDGE_CURVE ( 'NONE', #17171, #9020, #14362, .T. ) ;
#4996 = ORIENTED_EDGE ( 'NONE', *, *, #17095, .T. ) ;
#4997 = ORIENTED_EDGE ( 'NONE', *, *, #13423, .F. ) ;
#4998 = VERTEX_POINT ( 'NONE', #1556 ) ;
#4999 =( GEOMETRIC_REPRESENTATION_CONTEXT ( 3 ) GLOBAL_UNCERTAINTY_ASSIGNED_CONTEXT ( ( #16918 ) ) GLOBAL_UNIT_ASSIGNED_CONTEXT ( ( #3480, #360, #4372 ) ) REPRESENTATION_CONTEXT ( 'NONE', 'WORKASPACE' ) );
#5000 = CARTESIAN_POINT ( 'NONE',  ( 20.99999999999996092, 0.000000000000000000, 35.00000000000000711 ) ) ;
#5001 = SURFACE_SIDE_STYLE ('',( #19211 ) ) ;
#5002 = AXIS2_PLACEMENT_3D ( 'NONE', #8218, #3582, #3787 ) ;
#5003 = VERTEX_POINT ( 'NONE', #7867 ) ;
#5004 = CARTESIAN_POINT ( 'NONE',  ( 0.000000000000000000, -3.000000000000000888, 0.000000000000000000 ) ) ;
#5005 = ORIENTED_EDGE ( 'NONE', *, *, #13421, .T. ) ;
#5006 = DIRECTION ( 'NONE',  ( -0.000000000000000000, 1.000000000000000000, -0.000000000000000000 ) ) ;
#5007 = FACE_OUTER_BOUND ( 'NONE', #3143, .T. ) ;
#5008 = DIRECTION ( 'NONE',  ( 0.000000000000000000, 0.000000000000000000, -1.000000000000000000 ) ) ;
#5009 = LINE ( 'NONE', #154, #3045 ) ;
#5010 = CARTESIAN_POINT ( 'NONE',  ( 78.48937290013661539, 80.91625508013694912, 250.0000000000000000 ) ) ;
#5011 = CARTESIAN_POINT ( 'NONE',  ( -1.831162533324883990, 38.61573685184089300, 9.323294315095141727 ) ) ;
#5012 = EDGE_CURVE ( 'NONE', #14814, #14706, #19367, .T. ) ;
#5013 = ORIENTED_EDGE ( 'NONE', *, *, #15577, .T. ) ;
#5014 = CARTESIAN_POINT ( 'NONE',  ( -23.00000000000000000, 0.000000000000000000, -36.99999999999999289 ) ) ;
#5015 = CARTESIAN_POINT ( 'NONE',  ( 40.00000000000003553, 3.000000000000000000, 20.00000000000000355 ) ) ;
#5016 = PRESENTATION_STYLE_ASSIGNMENT (( #14785 ) ) ;
#5017 = STYLED_ITEM ( 'NONE', ( #10251 ), #17816 ) ;
#5018 = LINE ( 'NONE', #9444, #10647 ) ;
#5019 =( LENGTH_UNIT ( ) NAMED_UNIT ( * ) SI_UNIT ( .MILLI., .METRE. ) );
#5020 = LINE ( 'NONE', #17467, #10964 ) ;
#5021 = ORIENTED_EDGE ( 'NONE', *, *, #14260, .F. ) ;
#5022 = ADVANCED_FACE ( 'NONE', ( #31 ), #545, .F. ) ;
#5023 = ORIENTED_EDGE ( 'NONE', *, *, #13393, .T. ) ;
#5024 =( GEOMETRIC_REPRESENTATION_CONTEXT ( 3 ) GLOBAL_UNCERTAINTY_ASSIGNED_CONTEXT ( ( #16485 ) ) GLOBAL_UNIT_ASSIGNED_CONTEXT ( ( #17685, #14786, #10062 ) ) REPRESENTATION_CONTEXT ( 'NONE', 'WORKASPACE' ) );
#5025 = MECHANICAL_DESIGN_GEOMETRIC_PRESENTATION_REPRESENTATION (  '', ( #2708 ), #4025 ) ;
#5026 = VERTEX_POINT ( 'NONE', #6950 ) ;
#5027 = ADVANCED_FACE ( 'NONE', ( #3545 ), #13140, .F. ) ;
#5028 = ORIENTED_EDGE ( 'NONE', *, *, #17306, .F. ) ;
#5029 = FACE_OUTER_BOUND ( 'NONE', #9601, .T. ) ;
#5030 = AXIS2_PLACEMENT_3D ( 'NONE', #12674, #10291, #4734 ) ;
#5031 = CARTESIAN_POINT ( 'NONE',  ( 31.81980515339464333, 11.00000000000000000, 35.11980515339463693 ) ) ;
#5032 = AXIS2_PLACEMENT_3D ( 'NONE', #10476, #13395, #16984 ) ;
#5033 = ORIENTED_EDGE ( 'NONE', *, *, #13892, .T. ) ;
#5034 = LINE ( 'NONE', #9455, #19244 ) ;
#5035 = COLOUR_RGB ( '', 0.09019608, 0.27058824, 0.51372549) ;
#5036 = ORIENTED_EDGE ( 'NONE', *, *, #11142, .T. ) ;
#5037 = DIRECTION ( 'NONE',  ( 0.000000000000000000, 0.000000000000000000, -1.000000000000000000 ) ) ;
#5038 = DIRECTION ( 'NONE',  ( 1.000000000000000000, 0.000000000000000000, 0.000000000000000000 ) ) ;
#5039 = VERTEX_POINT ( 'NONE', #8026 ) ;
#5040 = DIRECTION ( 'NONE',  ( 0.000000000000000000, 0.000000000000000000, 1.000000000000000000 ) ) ;
#5041 = DIRECTION ( 'NONE',  ( -9.815121534730717399E-17, 1.000000000000000000, -2.352167425053297897E-16 ) ) ;
#5042 = CARTESIAN_POINT ( 'NONE',  ( 0.000000000000000000, 0.000000000000000000, 0.000000000000000000 ) ) ;
#5043 = PRESENTATION_STYLE_ASSIGNMENT (( #17237 ) ) ;
#5044 = CARTESIAN_POINT ( 'NONE',  ( 6.649999999999999467, 0.000000000000000000, 0.000000000000000000 ) ) ;
#5045 = CARTESIAN_POINT ( 'NONE',  ( 82.88953019741013861, 80.91625508013694912, 245.0000000000000000 ) ) ;
#5046 = PLANE ( 'NONE',  #6959 ) ;
#5047 = CONICAL_SURFACE ( 'NONE', #14235, 14.43750000000000000, 0.7483780475235185525 ) ;
#5048 =( GEOMETRIC_REPRESENTATION_CONTEXT ( 3 ) GLOBAL_UNCERTAINTY_ASSIGNED_CONTEXT ( ( #13810 ) ) GLOBAL_UNIT_ASSIGNED_CONTEXT ( ( #8162, #18307, #16691 ) ) REPRESENTATION_CONTEXT ( 'NONE', 'WORKASPACE' ) );
#5049 = ADVANCED_FACE ( 'NONE', ( #5201 ), #3854, .F. ) ;
#5050 = EDGE_LOOP ( 'NONE', ( #14108, #6176, #46, #19543 ) ) ;
#5051 = UNCERTAINTY_MEASURE_WITH_UNIT (LENGTH_MEASURE( 1.000000000000000082E-05 ), #7262, 'distance_accuracy_value', 'NONE');
#5052 = MECHANICAL_DESIGN_GEOMETRIC_PRESENTATION_REPRESENTATION (  '', ( #2392 ), #10307 ) ;
#5053 = CARTESIAN_POINT ( 'NONE',  ( -1.000000000000000888, 152.4824555358011082, 477.3411705753777596 ) ) ;
#5054 = VERTEX_POINT ( 'NONE', #5500 ) ;
#5055 = AXIS2_PLACEMENT_3D ( 'NONE', #9557, #3071, #11113 ) ;
#5056 = ORIENTED_EDGE ( 'NONE', *, *, #16807, .T. ) ;
#5057 = ORIENTED_EDGE ( 'NONE', *, *, #642, .F. ) ;
#5058 = DIRECTION ( 'NONE',  ( 0.000000000000000000, 1.000000000000000000, -0.000000000000000000 ) ) ;
#5059 = FACE_OUTER_BOUND ( 'NONE', #11533, .T. ) ;
#5060 = DIRECTION ( 'NONE',  ( 1.000000000000000000, 0.000000000000000000, 0.000000000000000000 ) ) ;
#5061 = CIRCLE ( 'NONE', #15925, 2.999999999999995559 ) ;
#5062 = CIRCLE ( 'NONE', #10315, 8.000000000000007105 ) ;
#5063 = DIRECTION ( 'NONE',  ( 0.000000000000000000, 0.000000000000000000, 1.000000000000000000 ) ) ;
#5064 = CARTESIAN_POINT ( 'NONE',  ( 3.500000000000000000, 0.000000000000000000, 0.000000000000000000 ) ) ;
#5065 = LINE ( 'NONE', #3520, #4377 ) ;
#5066 = DIRECTION ( 'NONE',  ( -0.000000000000000000, -0.000000000000000000, 1.000000000000000000 ) ) ;
#5067 = EDGE_CURVE ( 'NONE', #14445, #18751, #10490, .T. ) ;
#5068 = SURFACE_STYLE_USAGE ( .BOTH. , #16020 ) ;
#5069 = DIRECTION ( 'NONE',  ( 1.000000000000000000, 0.000000000000000000, 0.000000000000000000 ) ) ;
#5070 = PRESENTATION_LAYER_ASSIGNMENT (  '', '', ( #4407 ) ) ;
#5071 = CARTESIAN_POINT ( 'NONE',  ( 53.48937290013658696, 126.1646452518344859, 322.0399576098686225 ) ) ;
#5072 = VECTOR ( 'NONE', #19431, 1000.000000000000000 ) ;
#5073 = AXIS2_PLACEMENT_3D ( 'NONE', #11789, #5694, #12092 ) ;
#5074 = VERTEX_POINT ( 'NONE', #11682 ) ;
#5075 = CIRCLE ( 'NONE', #14290, 1.000000000000015987 ) ;
#5076 = EDGE_CURVE ( 'NONE', #1949, #4860, #6645, .T. ) ;
#5077 =( NAMED_UNIT ( * ) SI_UNIT ( $, .STERADIAN. ) SOLID_ANGLE_UNIT ( ) );
#5078 = EDGE_LOOP ( 'NONE', ( #7808, #19375, #12002, #12790, #3755, #5711 ) ) ;
#5079 = COLOUR_RGB ( '', 0.40784314, 0.44705882, 0.49803922) ;
#5080 = CARTESIAN_POINT ( 'NONE',  ( 2.625000000000000000, 0.000000000000000000, 0.000000000000000000 ) ) ;
#5081 = ORIENTED_EDGE ( 'NONE', *, *, #18566, .T. ) ;
#5082 = CARTESIAN_POINT ( 'NONE',  ( -211.5106270998635409, 113.1299228374912502, 220.6387154965113382 ) ) ;
#5083 = VERTEX_POINT ( 'NONE', #19591 ) ;
#5084 = MECHANICAL_DESIGN_GEOMETRIC_PRESENTATION_REPRESENTATION (  '', ( #14626 ), #7060 ) ;
#5085 = CARTESIAN_POINT ( 'NONE',  ( -78.99999999999995737, 216.7545334744432921, 510.3921618609452935 ) ) ;
#5086 = FILL_AREA_STYLE ('',( #8073 ) ) ;
#5087 = PLANE ( 'NONE',  #5369 ) ;
#5088 = ADVANCED_FACE ( 'NONE', ( #14557 ), #19390, .F. ) ;
#5089 = CIRCLE ( 'NONE', #6074, 36.50000000000000000 ) ;
#5090 = LINE ( 'NONE', #18041, #16337 ) ;
#5091 = CARTESIAN_POINT ( 'NONE',  ( -78.99999999949856999, 139.1140930665133908, 488.5333147763630564 ) ) ;
#5092 = AXIS2_PLACEMENT_3D ( 'NONE', #12155, #18428, #1101 ) ;
#5093 = CARTESIAN_POINT ( 'NONE',  ( 40.00000000000003553, 0.000000000000000000, 20.00000000000000355 ) ) ;
#5094 = VERTEX_POINT ( 'NONE', #17959 ) ;
#5095 = FILL_AREA_STYLE_COLOUR ( '', #3274 ) ;
#5096 = EDGE_CURVE ( 'NONE', #14619, #19590, #924, .T. ) ;
#5097 = LINE ( 'NONE', #16042, #18437 ) ;
#5098 = DIRECTION ( 'NONE',  ( 0.000000000000000000, 0.000000000000000000, -1.000000000000000000 ) ) ;
#5099 = AXIS2_PLACEMENT_3D ( 'NONE', #3509, #16101, #10112 ) ;
#5100 = VERTEX_POINT ( 'NONE', #16238 ) ;
#5101 = AXIS2_PLACEMENT_3D ( 'NONE', #8128, #15555, #8015 ) ;
#5102 = DIRECTION ( 'NONE',  ( -0.000000000000000000, -1.000000000000000000, -0.000000000000000000 ) ) ;
#5103 = ORIENTED_EDGE ( 'NONE', *, *, #14065, .T. ) ;
#5104 =( GEOMETRIC_REPRESENTATION_CONTEXT ( 3 ) GLOBAL_UNCERTAINTY_ASSIGNED_CONTEXT ( ( #13366 ) ) GLOBAL_UNIT_ASSIGNED_CONTEXT ( ( #3122, #17741, #6940 ) ) REPRESENTATION_CONTEXT ( 'NONE', 'WORKASPACE' ) );
#5105 = VERTEX_POINT ( 'NONE', #10035 ) ;
#5106 = EDGE_CURVE ( 'NONE', #15013, #3589, #15105, .T. ) ;
#5107 = EDGE_CURVE ( 'NONE', #14489, #9471, #16346, .T. ) ;
#5108 = ORIENTED_EDGE ( 'NONE', *, *, #11643, .F. ) ;
#5109 = VECTOR ( 'NONE', #125, 1000.000000000000000 ) ;
#5110 = ORIENTED_EDGE ( 'NONE', *, *, #12544, .F. ) ;
#5111 = AXIS2_PLACEMENT_3D ( 'NONE', #8445, #14409, #14613 ) ;
#5112 = DIRECTION ( 'NONE',  ( -0.000000000000000000, -1.000000000000000000, 0.000000000000000000 ) ) ;
#5113 = ADVANCED_FACE ( 'NONE', ( #14673, #8569, #14867 ), #19194, .T. ) ;
#5114 = ORIENTED_EDGE ( 'NONE', *, *, #11309, .F. ) ;
#5115 =( NAMED_UNIT ( * ) SI_UNIT ( $, .STERADIAN. ) SOLID_ANGLE_UNIT ( ) );
#5116 = CARTESIAN_POINT ( 'NONE',  ( 0.1087494598660525141, 139.9047507171206917, 489.0363018669112876 ) ) ;
#5117 = EDGE_LOOP ( 'NONE', ( #5596, #16541, #19394, #14597, #18988, #14183, #16328, #13903, #670, #8410, #7186, #11478 ) ) ;
#5118 = ADVANCED_FACE ( 'NONE', ( #20097 ), #7249, .T. ) ;
#5119 = LINE ( 'NONE', #2195, #18211 ) ;
#5120 = VECTOR ( 'NONE', #19975, 1000.000000000000000 ) ;
#5121 = DIRECTION ( 'NONE',  ( -1.000000000000000000, -0.000000000000000000, -0.000000000000000000 ) ) ;
#5122 = VECTOR ( 'NONE', #9524, 1000.000000000000000 ) ;
#5123 = AXIS2_PLACEMENT_3D ( 'NONE', #20277, #10709, #4526 ) ;
#5124 = PRESENTATION_STYLE_ASSIGNMENT (( #11488 ) ) ;
#5125 = CARTESIAN_POINT ( 'NONE',  ( -20.00000000000003197, 3.000000000000000000, 37.00000000000000711 ) ) ;
#5126 = PLANE ( 'NONE',  #18396 ) ;
#5127 = FACE_OUTER_BOUND ( 'NONE', #14151, .T. ) ;
#5128 = ORIENTED_EDGE ( 'NONE', *, *, #11262, .T. ) ;
#5129 = CARTESIAN_POINT ( 'NONE',  ( 1.347066989204613998E-15, -1.203706215242022682E-32, 24.99999999999999645 ) ) ;
#5130 = ADVANCED_FACE ( 'NONE', ( #16930 ), #1217, .F. ) ;
#5131 =( GEOMETRIC_REPRESENTATION_CONTEXT ( 3 ) GLOBAL_UNCERTAINTY_ASSIGNED_CONTEXT ( ( #8472 ) ) GLOBAL_UNIT_ASSIGNED_CONTEXT ( ( #10032, #7158, #18141 ) ) REPRESENTATION_CONTEXT ( 'NONE', 'WORKASPACE' ) );
#5132 = FILL_AREA_STYLE ('',( #3476 ) ) ;
#5133 =( NAMED_UNIT ( * ) PLANE_ANGLE_UNIT ( ) SI_UNIT ( $, .RADIAN. ) );
#5134 = AXIS2_PLACEMENT_3D ( 'NONE', #5642, #11835, #16585 ) ;
#5135 = AXIS2_PLACEMENT_3D ( 'NONE', #6253, #12530, #18794 ) ;
#5136 = ORIENTED_EDGE ( 'NONE', *, *, #7859, .T. ) ;
#5137 = DIRECTION ( 'NONE',  ( -0.000000000000000000, -0.000000000000000000, 1.000000000000000000 ) ) ;
#5138 = ORIENTED_EDGE ( 'NONE', *, *, #1293, .F. ) ;
#5139 = VECTOR ( 'NONE', #13836, 1000.000000000000000 ) ;
#5140 = EDGE_CURVE ( 'NONE', #17794, #7206, #13625, .T. ) ;
#5141 = VERTEX_POINT ( 'NONE', #10438 ) ;
#5142 = AXIS2_PLACEMENT_3D ( 'NONE', #2423, #20312, #18081 ) ;
#5143 = ORIENTED_EDGE ( 'NONE', *, *, #13900, .F. ) ;
#5144 = DIRECTION ( 'NONE',  ( 0.000000000000000000, 0.000000000000000000, -1.000000000000000000 ) ) ;
#5145 = ORIENTED_EDGE ( 'NONE', *, *, #13100, .T. ) ;
#5146 = CARTESIAN_POINT ( 'NONE',  ( 10.00000000000000000, 376.0487089519837127, -155.0000000000033253 ) ) ;
#5147 = ORIENTED_EDGE ( 'NONE', *, *, #8164, .F. ) ;
#5148 = EDGE_CURVE ( 'NONE', #10328, #10073, #18394, .T. ) ;
#5149 = DIRECTION ( 'NONE',  ( -1.000000000000000000, 0.000000000000000000, -8.673617379884027583E-16 ) ) ;
#5150 = FACE_OUTER_BOUND ( 'NONE', #12766, .T. ) ;
#5151 = AXIS2_PLACEMENT_3D ( 'NONE', #11565, #4158, #17948 ) ;
#5152 = DIRECTION ( 'NONE',  ( 0.000000000000000000, 0.000000000000000000, 1.000000000000000000 ) ) ;
#5153 = CARTESIAN_POINT ( 'NONE',  ( 0.000000000000000000, 38.00000000000000711, -5.741599279633704455E-16 ) ) ;
#5154 = CARTESIAN_POINT ( 'NONE',  ( 55.48937290013660117, 129.7247684487574588, 368.0000000000000000 ) ) ;
#5155 = EDGE_CURVE ( 'NONE', #758, #4994, #17749, .T. ) ;
#5156 = AXIS2_PLACEMENT_3D ( 'NONE', #1977, #12948, #5793 ) ;
#5157 =( NAMED_UNIT ( * ) SI_UNIT ( $, .STERADIAN. ) SOLID_ANGLE_UNIT ( ) );
#5158 = LINE ( 'NONE', #6811, #8404 ) ;
#5159 = FACE_OUTER_BOUND ( 'NONE', #1520, .T. ) ;
#5160 = CARTESIAN_POINT ( 'NONE',  ( -26.00000000000001776, 8.000000000000000000, 33.00000000000000711 ) ) ;
#5161 = DIRECTION ( 'NONE',  ( 0.000000000000000000, 0.000000000000000000, 1.000000000000000000 ) ) ;
#5162 =( LENGTH_UNIT ( ) NAMED_UNIT ( * ) SI_UNIT ( .MILLI., .METRE. ) );
#5163 = VERTEX_POINT ( 'NONE', #13732 ) ;
#5164 = ORIENTED_EDGE ( 'NONE', *, *, #18076, .F. ) ;
#5165 = VERTEX_POINT ( 'NONE', #19993 ) ;
#5166 = ORIENTED_EDGE ( 'NONE', *, *, #3685, .F. ) ;
#5167 = ORIENTED_EDGE ( 'NONE', *, *, #2246, .T. ) ;
#5168 = LINE ( 'NONE', #19039, #15359 ) ;
#5169 = DIRECTION ( 'NONE',  ( 0.000000000000000000, 1.000000000000000000, -0.000000000000000000 ) ) ;
#5170 = PRESENTATION_STYLE_ASSIGNMENT (( #8540 ) ) ;
#5171 = CARTESIAN_POINT ( 'NONE',  ( 10.00000000000000000, 372.8685141053783241, -146.8198051533979935 ) ) ;
#5172 = PRODUCT ( 'Part13^Assem2', 'Part13^Assem2', '', ( #2820 ) ) ;
#5173 = CARTESIAN_POINT ( 'NONE',  ( 1.750000000000000000, 0.000000000000000000, 0.000000000000000000 ) ) ;
#5174 = ADVANCED_FACE ( 'NONE', ( #5900 ), #10631, .T. ) ;
#5175 = DIRECTION ( 'NONE',  ( -6.123031769111888756E-17, 1.000000000000000000, 3.749151804555344967E-33 ) ) ;
#5176 = FACE_OUTER_BOUND ( 'NONE', #8034, .T. ) ;
#5177 = CARTESIAN_POINT ( 'NONE',  ( -22.99999999999999645, 68.00000000000000000, -31.00000000000005684 ) ) ;
#5178 = PLANE ( 'NONE',  #8909 ) ;
#5179 = DIRECTION ( 'NONE',  ( 0.000000000000000000, -0.000000000000000000, 1.000000000000000000 ) ) ;
#5180 = CARTESIAN_POINT ( 'NONE',  ( 463.8334540492693350, 191.8198460455371333, 225.0057801310552463 ) ) ;
#5181 = LINE ( 'NONE', #2248, #8699 ) ;
#5182 = VECTOR ( 'NONE', #4091, 1000.000000000000000 ) ;
#5183 = EDGE_LOOP ( 'NONE', ( #3976, #9048, #17013, #5325 ) ) ;
#5184 = CARTESIAN_POINT ( 'NONE',  ( -30.99999999999999645, 0.000000000000000000, -30.99999999999999289 ) ) ;
#5185 = UNCERTAINTY_MEASURE_WITH_UNIT (LENGTH_MEASURE( 1.000000000000000082E-05 ), #6722, 'distance_accuracy_value', 'NONE');
#5186 = ORIENTED_EDGE ( 'NONE', *, *, #20034, .F. ) ;
#5187 = FACE_BOUND ( 'NONE', #944, .T. ) ;
#5188 = EDGE_LOOP ( 'NONE', ( #6244, #315, #16246, #11696 ) ) ;
#5189 = UNCERTAINTY_MEASURE_WITH_UNIT (LENGTH_MEASURE( 1.000000000000000082E-05 ), #19529, 'distance_accuracy_value', 'NONE');
#5190 = CARTESIAN_POINT ( 'NONE',  ( 40.00000000000000711, 19.00000000000000000, 25.99999999999999645 ) ) ;
#5191 = DIRECTION ( 'NONE',  ( 0.000000000000000000, 0.000000000000000000, -1.000000000000000000 ) ) ;
#5192 = UNCERTAINTY_MEASURE_WITH_UNIT (LENGTH_MEASURE( 1.000000000000000082E-05 ), #13425, 'distance_accuracy_value', 'NONE');
#5193 = ORIENTED_EDGE ( 'NONE', *, *, #7913, .T. ) ;
#5194 = PRESENTATION_STYLE_ASSIGNMENT (( #229 ) ) ;
#5195 = ADVANCED_FACE ( 'NONE', ( #20204 ), #5248, .F. ) ;
#5196 = DIRECTION ( 'NONE',  ( -0.000000000000000000, -0.000000000000000000, 1.000000000000000000 ) ) ;
#5197 = SURFACE_STYLE_FILL_AREA ( #17953 ) ;
#5198 =( LENGTH_UNIT ( ) NAMED_UNIT ( * ) SI_UNIT ( .MILLI., .METRE. ) );
#5199 = SURFACE_STYLE_FILL_AREA ( #17245 ) ;
#5200 = ORIENTED_EDGE ( 'NONE', *, *, #16170, .T. ) ;
#5201 = FACE_OUTER_BOUND ( 'NONE', #15260, .T. ) ;
#5202 = LINE ( 'NONE', #4017, #19099 ) ;
#5203 = FACE_OUTER_BOUND ( 'NONE', #19235, .T. ) ;
#5204 = CARTESIAN_POINT ( 'NONE',  ( 0.000000000000000000, 372.8685141053778693, -83.18019484660869978 ) ) ;
#5205 = VERTEX_POINT ( 'NONE', #8339 ) ;
#5206 = ORIENTED_EDGE ( 'NONE', *, *, #20213, .T. ) ;
#5207 = EDGE_CURVE ( 'NONE', #18687, #11894, #9782, .T. ) ;
#5208 = ORIENTED_EDGE ( 'NONE', *, *, #18040, .F. ) ;
#5209 = CARTESIAN_POINT ( 'NONE',  ( -38.50085094405407204, 209.4098724938429541, 510.3921618609452935 ) ) ;
#5210 = VERTEX_POINT ( 'NONE', #17612 ) ;
#5211 = UNCERTAINTY_MEASURE_WITH_UNIT (LENGTH_MEASURE( 1.000000000000000082E-05 ), #3522, 'distance_accuracy_value', 'NONE');
#5212 = SURFACE_STYLE_USAGE ( .BOTH. , #10050 ) ;
#5213 = CARTESIAN_POINT ( 'NONE',  ( 0.7241137275630746828, 139.7735476527001879, 489.5362968091732796 ) ) ;
#5214 = EDGE_LOOP ( 'NONE', ( #19720, #13469, #2382, #5927 ) ) ;
#5215 =( NAMED_UNIT ( * ) PLANE_ANGLE_UNIT ( ) SI_UNIT ( $, .RADIAN. ) );
#5216 = CYLINDRICAL_SURFACE ( 'NONE', #15237, 2.000000000000001776 ) ;
#5217 = AXIS2_PLACEMENT_3D ( 'NONE', #5637, #6162, #10680 ) ;
#5218 = EDGE_CURVE ( 'NONE', #5765, #3170, #497, .T. ) ;
#5219 = DIRECTION ( 'NONE',  ( 0.000000000000000000, 0.000000000000000000, 1.000000000000000000 ) ) ;
#5220 = VERTEX_POINT ( 'NONE', #11212 ) ;
#5221 = DIRECTION ( 'NONE',  ( 0.000000000000000000, -1.000000000000000000, 0.000000000000000000 ) ) ;
#5222 = DIRECTION ( 'NONE',  ( -1.000000000000000000, 0.000000000000000000, 0.000000000000000000 ) ) ;
#5223 = SURFACE_STYLE_FILL_AREA ( #5425 ) ;
#5224 = SHAPE_REPRESENTATION_RELATIONSHIP ( 'NONE' , 'NONE' ,  #4054, #17238 ) ;
#5225 = ORIENTED_EDGE ( 'NONE', *, *, #10154, .T. ) ;
#5226 = EDGE_CURVE ( 'NONE', #1243, #16197, #16092, .T. ) ;
#5227 = DIRECTION ( 'NONE',  ( 1.000000000000000000, 0.000000000000000000, -0.000000000000000000 ) ) ;
#5228 = ORIENTED_EDGE ( 'NONE', *, *, #1826, .T. ) ;
#5229 = AXIS2_PLACEMENT_3D ( 'NONE', #16451, #6784, #19701 ) ;
#5230 = ORIENTED_EDGE ( 'NONE', *, *, #17733, .T. ) ;
#5231 = EDGE_CURVE ( 'NONE', #12661, #16049, #18663, .T. ) ;
#5232 = EDGE_LOOP ( 'NONE', ( #4898, #3553, #4873, #11660 ) ) ;
#5233 = CARTESIAN_POINT ( 'NONE',  ( 78.48937290013660117, 123.1299228374914208, 220.6387154965113382 ) ) ;
#5234 = EDGE_CURVE ( 'NONE', #19951, #5831, #2249, .T. ) ;
#5235 = CARTESIAN_POINT ( 'NONE',  ( 0.000000000000000000, 372.8685141053778693, -79.88019484660868841 ) ) ;
#5236 = ORIENTED_EDGE ( 'NONE', *, *, #19210, .T. ) ;
#5237 = LINE ( 'NONE', #11510, #5435 ) ;
#5238 = VERTEX_POINT ( 'NONE', #12779 ) ;
#5239 = DIRECTION ( 'NONE',  ( 0.000000000000000000, 0.000000000000000000, 1.000000000000000000 ) ) ;
#5240 = DIRECTION ( 'NONE',  ( -0.000000000000000000, -1.000000000000000000, -0.000000000000000000 ) ) ;
#5241 = CARTESIAN_POINT ( 'NONE',  ( 111.4893729001366012, 129.7247684487574588, 368.0000000000000000 ) ) ;
#5242 = ADVANCED_FACE ( 'NONE', ( #11428 ), #3601, .T. ) ;
#5243 = PRESENTATION_LAYER_ASSIGNMENT (  '', '', ( #6900 ) ) ;
#5244 = CARTESIAN_POINT ( 'NONE',  ( 0.000000000000000000, 216.7545334744432921, 495.1946179577816451 ) ) ;
#5245 = CARTESIAN_POINT ( 'NONE',  ( 0.6999999999999999556, 0.000000000000000000, 0.000000000000000000 ) ) ;
#5246 = FACE_OUTER_BOUND ( 'NONE', #1343, .T. ) ;
#5247 = DIRECTION ( 'NONE',  ( 0.000000000000000000, 1.000000000000000000, 0.000000000000000000 ) ) ;
#5248 = PLANE ( 'NONE',  #15793 ) ;
#5249 = ORIENTED_EDGE ( 'NONE', *, *, #324, .F. ) ;
#5250 = CARTESIAN_POINT ( 'NONE',  ( -19.00000000000001776, 8.000000000000000000, 40.00000000000000711 ) ) ;
#5251 = ORIENTED_EDGE ( 'NONE', *, *, #17441, .F. ) ;
#5252 = EDGE_CURVE ( 'NONE', #7117, #2094, #11317, .T. ) ;
#5253 = EDGE_CURVE ( 'NONE', #19516, #3677, #2993, .T. ) ;
#5254 = CIRCLE ( 'NONE', #4597, 12.00000000000000178 ) ;
#5255 = ORIENTED_EDGE ( 'NONE', *, *, #5949, .T. ) ;
#5256 = AXIS2_PLACEMENT_3D ( 'NONE', #285, #17707, #14040 ) ;
#5257 = MECHANICAL_DESIGN_GEOMETRIC_PRESENTATION_REPRESENTATION (  '', ( #9189 ), #20032 ) ;
#5258 = ORIENTED_EDGE ( 'NONE', *, *, #15417, .T. ) ;
#5259 = ORIENTED_EDGE ( 'NONE', *, *, #8810, .T. ) ;
#5260 = CARTESIAN_POINT ( 'NONE',  ( 7.000000000000000000, 0.000000000000000000, 0.000000000000000000 ) ) ;
#5261 = CARTESIAN_POINT ( 'NONE',  ( 78.48937290013660117, 145.9162550801369491, 0.000000000000000000 ) ) ;
#5262 = DIRECTION ( 'NONE',  ( 1.000000000000000000, -0.000000000000000000, 0.000000000000000000 ) ) ;
#5263 = CARTESIAN_POINT ( 'NONE',  ( 36.99999999999999289, 10.00000000000000000, 17.99999999999998934 ) ) ;
#5264 = FACE_OUTER_BOUND ( 'NONE', #5699, .T. ) ;
#5265 = DIRECTION ( 'NONE',  ( 0.000000000000000000, 0.7071067811865336949, 0.7071067811865614505 ) ) ;
#5266 = FILL_AREA_STYLE ('',( #16408 ) ) ;
#5267 = DIRECTION ( 'NONE',  ( 0.000000000000000000, 1.000000000000000000, 0.000000000000000000 ) ) ;
#5268 = APPLICATION_CONTEXT ( 'automotive_design' ) ;
#5269 = SURFACE_STYLE_USAGE ( .BOTH. , #3620 ) ;
#5270 = AXIS2_PLACEMENT_3D ( 'NONE', #4929, #9969, #1824 ) ;
#5271 = CARTESIAN_POINT ( 'NONE',  ( 423.8334540492694487, 191.8198460455371333, 24.99421986894476078 ) ) ;
#5272 = AXIS2_PLACEMENT_3D ( 'NONE', #3958, #10053, #2194 ) ;
#5273 = EDGE_CURVE ( 'NONE', #6469, #10221, #9877, .T. ) ;
#5274 = CARTESIAN_POINT ( 'NONE',  ( 35.99999999999999289, 8.000000000000000000, 21.99999999999999645 ) ) ;
#5275 = DIRECTION ( 'NONE',  ( -0.000000000000000000, -1.000000000000000000, 0.000000000000000000 ) ) ;
#5276 = EDGE_CURVE ( 'NONE', #15939, #12917, #16777, .T. ) ;
#5277 = ORIENTED_EDGE ( 'NONE', *, *, #16074, .T. ) ;
#5278 = CARTESIAN_POINT ( 'NONE',  ( 0.000000000000000000, 139.4861549369088323, 500.2186618848270996 ) ) ;
#5279 = VERTEX_POINT ( 'NONE', #4936 ) ;
#5280 = MECHANICAL_DESIGN_GEOMETRIC_PRESENTATION_REPRESENTATION (  '', ( #11540 ), #7906 ) ;
#5281 = VECTOR ( 'NONE', #16575, 1000.000000000000000 ) ;
#5282 = ORIENTED_EDGE ( 'NONE', *, *, #181, .F. ) ;
#5283 = AXIS2_PLACEMENT_3D ( 'NONE', #2508, #19794, #5703 ) ;
#5284 = SURFACE_STYLE_FILL_AREA ( #11665 ) ;
#5285 = ORIENTED_EDGE ( 'NONE', *, *, #11923, .F. ) ;
#5286 = DIRECTION ( 'NONE',  ( -1.000000000000000000, 0.000000000000000000, -1.135258727068399668E-15 ) ) ;
#5287 = DIRECTION ( 'NONE',  ( 0.000000000000000000, 0.000000000000000000, 1.000000000000000000 ) ) ;
#5288 = ORIENTED_EDGE ( 'NONE', *, *, #5106, .F. ) ;
#5289 =( NAMED_UNIT ( * ) SI_UNIT ( $, .STERADIAN. ) SOLID_ANGLE_UNIT ( ) );
#5290 = CARTESIAN_POINT ( 'NONE',  ( 0.000000000000000000, 0.000000000000000000, 0.000000000000000000 ) ) ;
#5291 = LINE ( 'NONE', #10218, #17855 ) ;
#5292 = DIRECTION ( 'NONE',  ( 6.123031769111888756E-17, 0.000000000000000000, 1.000000000000000000 ) ) ;
#5293 = DIRECTION ( 'NONE',  ( 0.000000000000000000, 0.000000000000000000, -1.000000000000000000 ) ) ;
#5294 = ORIENTED_EDGE ( 'NONE', *, *, #3201, .F. ) ;
#5295 = DIRECTION ( 'NONE',  ( 1.000000000000000000, 5.889072920838430686E-16, -0.000000000000000000 ) ) ;
#5296 = CARTESIAN_POINT ( 'NONE',  ( 1.181929469892510243, 216.7545334744432921, 490.5655098179833544 ) ) ;
#5297 = DIRECTION ( 'NONE',  ( -1.000000000000000000, 0.000000000000000000, -0.000000000000000000 ) ) ;
#5298 = AXIS2_PLACEMENT_3D ( 'NONE', #20172, #9462, #14203 ) ;
#5299 = CONTEXT_DEPENDENT_SHAPE_REPRESENTATION ( #9185, #12902 ) ;
#5300 = VECTOR ( 'NONE', #15950, 1000.000000000000000 ) ;
#5301 = AXIS2_PLACEMENT_3D ( 'NONE', #10128, #19479, #13045 ) ;
#5302 = ORIENTED_EDGE ( 'NONE', *, *, #6342, .F. ) ;
#5303 = EDGE_CURVE ( 'NONE', #7139, #6891, #19383, .T. ) ;
#5304 = VECTOR ( 'NONE', #8360, 1000.000000000000114 ) ;
#5305 = ORIENTED_EDGE ( 'NONE', *, *, #15207, .T. ) ;
#5306 = EDGE_LOOP ( 'NONE', ( #16374, #20359, #15838, #16965 ) ) ;
#5307 = DIRECTION ( 'NONE',  ( 0.000000000000000000, 1.000000000000000000, 0.000000000000000000 ) ) ;
#5308 = ORIENTED_EDGE ( 'NONE', *, *, #7423, .T. ) ;
#5309 = DIRECTION ( 'NONE',  ( 0.000000000000000000, 0.000000000000000000, 1.000000000000000000 ) ) ;
#5310 = VECTOR ( 'NONE', #2869, 1000.000000000000000 ) ;
#5311 = CARTESIAN_POINT ( 'NONE',  ( 2.601523022692213694, 39.49322514888784497, 9.137549538570182150 ) ) ;
#5312 = VERTEX_POINT ( 'NONE', #2017 ) ;
#5313 = MECHANICAL_DESIGN_GEOMETRIC_PRESENTATION_REPRESENTATION (  '', ( #15839 ), #3978 ) ;
#5314 = PRESENTATION_STYLE_ASSIGNMENT (( #19313 ) ) ;
#5315 = DIRECTION ( 'NONE',  ( -0.000000000000000000, -1.000000000000000000, -0.000000000000000000 ) ) ;
#5316 = SURFACE_STYLE_FILL_AREA ( #8709 ) ;
#5317 = DIRECTION ( 'NONE',  ( 1.000000000000000000, 9.815121534730717399E-17, 0.000000000000000000 ) ) ;
#5318 = DIRECTION ( 'NONE',  ( 1.000000000000000000, 2.135044278125300850E-16, -0.000000000000000000 ) ) ;
#5319 = VERTEX_POINT ( 'NONE', #8236 ) ;
#5320 = SURFACE_SIDE_STYLE ('',( #19411 ) ) ;
#5321 = CARTESIAN_POINT ( 'NONE',  ( -34.99999999999996447, 8.000000000000000000, -40.00000000000000711 ) ) ;
#5322 = EDGE_CURVE ( 'NONE', #12613, #9677, #10507, .T. ) ;
#5323 = EDGE_LOOP ( 'NONE', ( #15311, #2163 ) ) ;
#5324 = DIRECTION ( 'NONE',  ( 1.000000000000000000, 0.000000000000000000, -1.322948291343117631E-12 ) ) ;
#5325 = ORIENTED_EDGE ( 'NONE', *, *, #7873, .F. ) ;
#5326 = CIRCLE ( 'NONE', #18455, 1.000000000000000888 ) ;
#5327 = PRESENTATION_LAYER_ASSIGNMENT (  '', '', ( #8941 ) ) ;
#5328 = ORIENTED_EDGE ( 'NONE', *, *, #15391, .T. ) ;
#5329 = EDGE_CURVE ( 'NONE', #1058, #2483, #4912, .T. ) ;
#5330 = VERTEX_POINT ( 'NONE', #1432 ) ;
#5331 = CARTESIAN_POINT ( 'NONE',  ( -75.00000000000000000, 368.2663108437010919, -142.2176018917206761 ) ) ;
#5332 = DIRECTION ( 'NONE',  ( 0.000000000000000000, 0.000000000000000000, -1.000000000000000000 ) ) ;
#5333 = ORIENTED_EDGE ( 'NONE', *, *, #2933, .T. ) ;
#5334 = CARTESIAN_POINT ( 'NONE',  ( 423.8334540492694487, 191.8198460455371333, 81.76606011801540319 ) ) ;
#5335 = EDGE_CURVE ( 'NONE', #17102, #17171, #381, .T. ) ;
#5336 = DIRECTION ( 'NONE',  ( 1.000000000000000000, -0.000000000000000000, 0.000000000000000000 ) ) ;
#5337 = DIRECTION ( 'NONE',  ( 0.000000000000000000, 0.000000000000000000, 1.000000000000000000 ) ) ;
#5338 = DIRECTION ( 'NONE',  ( 1.000000000000000000, -0.000000000000000000, -0.000000000000000000 ) ) ;
#5339 = CYLINDRICAL_SURFACE ( 'NONE', #13627, 1.000000000000000888 ) ;
#5340 = AXIS2_PLACEMENT_3D ( 'NONE', #8437, #16179, #3792 ) ;
#5341 = CARTESIAN_POINT ( 'NONE',  ( -31.81980515339462912, 0.000000000000000000, -35.11980515339465114 ) ) ;
#5342 =( LENGTH_UNIT ( ) NAMED_UNIT ( * ) SI_UNIT ( .MILLI., .METRE. ) );
#5343 = FACE_BOUND ( 'NONE', #2230, .T. ) ;
#5344 = DIRECTION ( 'NONE',  ( -0.000000000000000000, -1.000000000000000000, 0.000000000000000000 ) ) ;
#5345 = ORIENTED_EDGE ( 'NONE', *, *, #14145, .F. ) ;
#5346 = FACE_OUTER_BOUND ( 'NONE', #5456, .T. ) ;
#5347 = CARTESIAN_POINT ( 'NONE',  ( -26.00000000000000000, 19.00000000000000000, 40.00000000000001421 ) ) ;
#5348 = EDGE_CURVE ( 'NONE', #14026, #20243, #14450, .T. ) ;
#5349 = ORIENTED_EDGE ( 'NONE', *, *, #5590, .F. ) ;
#5350 = ORIENTED_EDGE ( 'NONE', *, *, #14596, .F. ) ;
#5351 = AXIS2_PLACEMENT_3D ( 'NONE', #9876, #12990, #2332 ) ;
#5352 = ORIENTED_EDGE ( 'NONE', *, *, #7113, .T. ) ;
#5353 = EDGE_CURVE ( 'NONE', #1341, #3236, #6593, .T. ) ;
#5354 = EDGE_LOOP ( 'NONE', ( #16645, #1779, #10978, #10701 ) ) ;
#5355 = ORIENTED_EDGE ( 'NONE', *, *, #10277, .T. ) ;
#5356 = CARTESIAN_POINT ( 'NONE',  ( 4.469960816887838430E-15, 50.00000000000000000, 36.50000000000000000 ) ) ;
#5357 = FACE_BOUND ( 'NONE', #3925, .T. ) ;
#5358 = DIRECTION ( 'NONE',  ( 0.000000000000000000, -1.000000000000000000, 0.000000000000000000 ) ) ;
#5359 = PRODUCT_DEFINITION_FORMATION_WITH_SPECIFIED_SOURCE ( 'ANY', '', #18958, .NOT_KNOWN. ) ;
#5360 = SURFACE_SIDE_STYLE ('',( #16106 ) ) ;
#5361 = PRESENTATION_LAYER_ASSIGNMENT (  '', '', ( #14232 ) ) ;
#5362 = EDGE_CURVE ( 'NONE', #1465, #5074, #1594, .T. ) ;
#5363 = VECTOR ( 'NONE', #10626, 1000.000000000000000 ) ;
#5364 = FACE_OUTER_BOUND ( 'NONE', #2050, .T. ) ;
#5365 = SURFACE_SIDE_STYLE ('',( #4009 ) ) ;
#5366 = ADVANCED_FACE ( 'NONE', ( #7201, #2333 ), #13399, .T. ) ;
#5367 = CARTESIAN_POINT ( 'NONE',  ( 0.1969510947806087375, 63.00000000000001421, 9.500000000000003553 ) ) ;
#5368 = DIRECTION ( 'NONE',  ( 0.000000000000000000, 1.000000000000000000, 0.000000000000000000 ) ) ;
#5369 = AXIS2_PLACEMENT_3D ( 'NONE', #15270, #7541, #12170 ) ;
#5370 = AXIS2_PLACEMENT_3D ( 'NONE', #7802, #4907, #6464 ) ;
#5371 = ADVANCED_FACE ( 'NONE', ( #16480 ), #883, .T. ) ;
#5372 = CARTESIAN_POINT ( 'NONE',  ( 20.99999999999996092, 0.000000000000000000, 37.50000000000001421 ) ) ;
#5373 = STYLED_ITEM ( 'NONE', ( #2632 ), #8230 ) ;
#5374 = EDGE_CURVE ( 'NONE', #7754, #10337, #19535, .T. ) ;
#5375 = CARTESIAN_POINT ( 'NONE',  ( 23.00000000000000711, 68.00000000000000000, -36.99999999999999289 ) ) ;
#5376 = SURFACE_STYLE_FILL_AREA ( #19460 ) ;
#5377 = VECTOR ( 'NONE', #12581, 1000.000000000000000 ) ;
#5378 = ORIENTED_EDGE ( 'NONE', *, *, #13284, .F. ) ;
#5379 = DIRECTION ( 'NONE',  ( 0.000000000000000000, 1.000000000000000000, 0.000000000000000000 ) ) ;
#5380 = UNCERTAINTY_MEASURE_WITH_UNIT (LENGTH_MEASURE( 1.000000000000000082E-05 ), #266, 'distance_accuracy_value', 'NONE');
#5381 = ORIENTED_EDGE ( 'NONE', *, *, #13828, .T. ) ;
#5382 = CIRCLE ( 'NONE', #6770, 10.00000000000000888 ) ;
#5383 = ORIENTED_EDGE ( 'NONE', *, *, #19025, .F. ) ;
#5384 = CARTESIAN_POINT ( 'NONE',  ( -40.00000000000000711, 0.000000000000000000, 26.00000000000000000 ) ) ;
#5385 = UNCERTAINTY_MEASURE_WITH_UNIT (LENGTH_MEASURE( 1.000000000000000082E-05 ), #10755, 'distance_accuracy_value', 'NONE');
#5386 = LINE ( 'NONE', #532, #656 ) ;
#5387 = VERTEX_POINT ( 'NONE', #19635 ) ;
#5388 = DIRECTION ( 'NONE',  ( -1.000000000000000000, 0.000000000000000000, 0.000000000000000000 ) ) ;
#5389 = DIRECTION ( 'NONE',  ( 1.000000000000000000, -0.000000000000000000, -0.000000000000000000 ) ) ;
#5390 = CARTESIAN_POINT ( 'NONE',  ( 498.8334540492693918, 214.2156642432025251, 0.000000000000000000 ) ) ;
#5391 = ADVANCED_FACE ( 'NONE', ( #17906 ), #10391, .F. ) ;
#5392 = DIRECTION ( 'NONE',  ( -1.000000000000000000, 0.000000000000000000, 0.000000000000000000 ) ) ;
#5393 = LINE ( 'NONE', #16132, #7019 ) ;
#5394 = CARTESIAN_POINT ( 'NONE',  ( -1.836909530733565148E-16, 6.000000000000000000, 3.000000000000000000 ) ) ;
#5395 = DIRECTION ( 'NONE',  ( -0.000000000000000000, -0.000000000000000000, 1.000000000000000000 ) ) ;
#5396 = EDGE_CURVE ( 'NONE', #17052, #14513, #14803, .T. ) ;
#5397 = ORIENTED_EDGE ( 'NONE', *, *, #12250, .T. ) ;
#5398 = SURFACE_SIDE_STYLE ('',( #11374 ) ) ;
#5399 = LINE ( 'NONE', #733, #4419 ) ;
#5400 = VECTOR ( 'NONE', #11617, 1000.000000000000000 ) ;
#5401 = MECHANICAL_DESIGN_GEOMETRIC_PRESENTATION_REPRESENTATION (  '', ( #2074 ), #1397 ) ;
#5402 = CARTESIAN_POINT ( 'NONE',  ( 153.4893729001366864, 113.1299228374914634, 29.36128450348865471 ) ) ;
#5403 = EDGE_CURVE ( 'NONE', #4354, #2287, #641, .T. ) ;
#5404 = AXIS2_PLACEMENT_3D ( 'NONE', #7515, #15139, #15244 ) ;
#5405 = VECTOR ( 'NONE', #14027, 1000.000000000000000 ) ;
#5406 = ORIENTED_EDGE ( 'NONE', *, *, #6541, .F. ) ;
#5407 = ORIENTED_EDGE ( 'NONE', *, *, #15220, .F. ) ;
#5408 = AXIS2_PLACEMENT_3D ( 'NONE', #12840, #19098, #14070 ) ;
#5409 = FACE_BOUND ( 'NONE', #1833, .T. ) ;
#5410 = ORIENTED_EDGE ( 'NONE', *, *, #2351, .T. ) ;
#5411 = CARTESIAN_POINT ( 'NONE',  ( 423.8334540492694487, 191.8198460455371333, 235.0057801310552463 ) ) ;
#5412 = STYLED_ITEM ( 'NONE', ( #540 ), #14853 ) ;
#5413 = VERTEX_POINT ( 'NONE', #3996 ) ;
#5414 = CARTESIAN_POINT ( 'NONE',  ( -33.00000000000000000, 8.000000000000000000, -22.00000000000000355 ) ) ;
#5415 =( GEOMETRIC_REPRESENTATION_CONTEXT ( 3 ) GLOBAL_UNCERTAINTY_ASSIGNED_CONTEXT ( ( #17941 ) ) GLOBAL_UNIT_ASSIGNED_CONTEXT ( ( #19896, #10632, #18260 ) ) REPRESENTATION_CONTEXT ( 'NONE', 'WORKASPACE' ) );
#5416 = FACE_OUTER_BOUND ( 'NONE', #15128, .T. ) ;
#5417 = SURFACE_STYLE_USAGE ( .BOTH. , #10056 ) ;
#5418 = LINE ( 'NONE', #17978, #7547 ) ;
#5419 = EDGE_CURVE ( 'NONE', #10868, #13471, #6906, .T. ) ;
#5420 = DIRECTION ( 'NONE',  ( 1.000000000000000000, 0.000000000000000000, 0.000000000000000000 ) ) ;
#5421 = AXIS2_PLACEMENT_3D ( 'NONE', #12063, #11948, #10488 ) ;
#5422 = ORIENTED_EDGE ( 'NONE', *, *, #19187, .T. ) ;
#5423 = FACE_OUTER_BOUND ( 'NONE', #8238, .T. ) ;
#5424 =( NAMED_UNIT ( * ) SI_UNIT ( $, .STERADIAN. ) SOLID_ANGLE_UNIT ( ) );
#5425 = FILL_AREA_STYLE ('',( #19414 ) ) ;
#5426 = DIRECTION ( 'NONE',  ( 1.000000000000000000, -3.491481338843170432E-15, -1.047444401652938744E-14 ) ) ;
#5427 = AXIS2_PLACEMENT_3D ( 'NONE', #14751, #8273, #14545 ) ;
#5428 = CARTESIAN_POINT ( 'NONE',  ( -41.50085094405408626, 209.4098724938429541, 505.3921618609452935 ) ) ;
#5429 = AXIS2_PLACEMENT_3D ( 'NONE', #16758, #19700, #14781 ) ;
#5430 = EDGE_LOOP ( 'NONE', ( #1615, #6034, #9826, #11300 ) ) ;
#5431 = COLOUR_RGB ( '', 0.66274510, 0.83137255, 0.94901961) ;
#5432 = COLOUR_RGB ( '', 0.31764706, 0.68627451, 0.89019608) ;
#5433 = EDGE_LOOP ( 'NONE', ( #16722, #7800, #17698, #15473 ) ) ;
#5434 = MECHANICAL_DESIGN_GEOMETRIC_PRESENTATION_REPRESENTATION (  '', ( #19558 ), #13993 ) ;
#5435 = VECTOR ( 'NONE', #9965, 1000.000000000000000 ) ;
#5436 = VERTEX_POINT ( 'NONE', #11622 ) ;
#5437 = ORIENTED_EDGE ( 'NONE', *, *, #12060, .F. ) ;
#5438 = CARTESIAN_POINT ( 'NONE',  ( -82.18192946989277914, 216.7545334744432921, 500.8237260975782874 ) ) ;
#5439 = VECTOR ( 'NONE', #1910, 1000.000000000000000 ) ;
#5440 = VERTEX_POINT ( 'NONE', #18002 ) ;
#5441 = DIRECTION ( 'NONE',  ( 0.000000000000000000, 0.000000000000000000, 1.000000000000000000 ) ) ;
#5442 = CARTESIAN_POINT ( 'NONE',  ( -80.99999999999995737, 216.7545334744432921, 501.8237260975782874 ) ) ;
#5443 = VECTOR ( 'NONE', #11902, 1000.000000000000227 ) ;
#5444 = DIRECTION ( 'NONE',  ( 0.000000000000000000, -1.000000000000000000, 0.000000000000000000 ) ) ;
#5445 = AXIS2_PLACEMENT_3D ( 'NONE', #10297, #10676, #8541 ) ;
#5446 = CARTESIAN_POINT ( 'NONE',  ( 3.850000000000000089, 0.000000000000000000, 0.000000000000000000 ) ) ;
#5447 = LINE ( 'NONE', #8335, #17365 ) ;
#5448 = DIRECTION ( 'NONE',  ( -0.000000000000000000, -1.000000000000000000, -0.000000000000000000 ) ) ;
#5449 = CARTESIAN_POINT ( 'NONE',  ( 32.99999999999998579, 8.000000000000000000, 25.99999999999999645 ) ) ;
#5450 = STYLED_ITEM ( 'NONE', ( #11890 ), #2091 ) ;
#5451 = DIRECTION ( 'NONE',  ( 1.000000000000000000, 0.000000000000000000, 0.000000000000000000 ) ) ;
#5452 = ORIENTED_EDGE ( 'NONE', *, *, #16949, .T. ) ;
#5453 = UNCERTAINTY_MEASURE_WITH_UNIT (LENGTH_MEASURE( 1.000000000000000082E-05 ), #20315, 'distance_accuracy_value', 'NONE');
#5454 = DIRECTION ( 'NONE',  ( -0.000000000000000000, -1.000000000000000000, -0.000000000000000000 ) ) ;
#5455 =( LENGTH_UNIT ( ) NAMED_UNIT ( * ) SI_UNIT ( .MILLI., .METRE. ) );
#5456 = EDGE_LOOP ( 'NONE', ( #18358, #5333, #18689, #14095 ) ) ;
#5457 = CIRCLE ( 'NONE', #12054, 14.59999999999999964 ) ;
#5458 = ORIENTED_EDGE ( 'NONE', *, *, #18566, .F. ) ;
#5459 = EDGE_LOOP ( 'NONE', ( #12514, #1199, #3493, #5548 ) ) ;
#5460 = EDGE_LOOP ( 'NONE', ( #9623, #6065, #3832, #9650 ) ) ;
#5461 = ADVANCED_FACE ( 'NONE', ( #16587 ), #13191, .F. ) ;
#5462 = SURFACE_SIDE_STYLE ('',( #8758 ) ) ;
#5463 = AXIS2_PLACEMENT_3D ( 'NONE', #18133, #10321, #2489 ) ;
#5464 = SURFACE_STYLE_USAGE ( .BOTH. , #8352 ) ;
#5465 = CARTESIAN_POINT ( 'NONE',  ( 53.48937290013659407, 145.9162550801369491, 0.000000000000000000 ) ) ;
#5466 = CARTESIAN_POINT ( 'NONE',  ( 19.99999999999995381, 3.000000000000000000, -39.99999999999999289 ) ) ;
#5467 = CARTESIAN_POINT ( 'NONE',  ( -18.00000000000001421, 6.000000000000000000, 40.00000000000000711 ) ) ;
#5468 = CIRCLE ( 'NONE', #18951, 3.299999999999997158 ) ;
#5469 = DIRECTION ( 'NONE',  ( 0.000000000000000000, 0.000000000000000000, 1.000000000000000000 ) ) ;
#5470 = CARTESIAN_POINT ( 'NONE',  ( -64.99999999999995737, 316.7545334744432353, 475.1454018718993098 ) ) ;
#5471 = CARTESIAN_POINT ( 'NONE',  ( -79.99999999999995737, 139.2066006846527841, 488.2525619656396429 ) ) ;
#5472 = SURFACE_STYLE_FILL_AREA ( #3524 ) ;
#5473 = ADVANCED_FACE ( 'NONE', ( #16392 ), #2226, .F. ) ;
#5474 = DIRECTION ( 'NONE',  ( 0.000000000000000000, 0.000000000000000000, -1.000000000000000000 ) ) ;
#5475 = VECTOR ( 'NONE', #16205, 1000.000000000000000 ) ;
#5476 = EDGE_CURVE ( 'NONE', #4581, #16084, #19840, .T. ) ;
#5477 = ORIENTED_EDGE ( 'NONE', *, *, #6739, .F. ) ;
#5478 = STYLED_ITEM ( 'NONE', ( #20157 ), #9624 ) ;
#5479 = EDGE_CURVE ( 'NONE', #19115, #9381, #18738, .T. ) ;
#5480 = ORIENTED_EDGE ( 'NONE', *, *, #7913, .F. ) ;
#5481 = FACE_BOUND ( 'NONE', #7482, .T. ) ;
#5482 = ORIENTED_EDGE ( 'NONE', *, *, #15181, .T. ) ;
#5483 = VERTEX_POINT ( 'NONE', #8930 ) ;
#5484 = EDGE_CURVE ( 'NONE', #7013, #3581, #12049, .T. ) ;
#5485 = ORIENTED_EDGE ( 'NONE', *, *, #1098, .T. ) ;
#5486 =( LENGTH_UNIT ( ) NAMED_UNIT ( * ) SI_UNIT ( .MILLI., .METRE. ) );
#5487 = LINE ( 'NONE', #16221, #6954 ) ;
#5488 = EDGE_CURVE ( 'NONE', #6229, #2111, #19942, .T. ) ;
#5489 =( NAMED_UNIT ( * ) PLANE_ANGLE_UNIT ( ) SI_UNIT ( $, .RADIAN. ) );
#5490 = VERTEX_POINT ( 'NONE', #15546 ) ;
#5491 = CARTESIAN_POINT ( 'NONE',  ( -211.5106270998635409, 103.1299228374912360, 220.6387154965113382 ) ) ;
#5492 = DIRECTION ( 'NONE',  ( -0.000000000000000000, -1.000000000000000000, -0.000000000000000000 ) ) ;
#5493 = CIRCLE ( 'NONE', #4506, 3.299999999999997158 ) ;
#5494 = CARTESIAN_POINT ( 'NONE',  ( -1.776356839400249676E-15, -13.94999999999999929, -1.708382284810557762E-15 ) ) ;
#5495 = FACE_OUTER_BOUND ( 'NONE', #15548, .T. ) ;
#5496 = DIRECTION ( 'NONE',  ( 0.7327934916262990317, -0.6804510993672779895, 8.333122608164345406E-17 ) ) ;
#5497 = SURFACE_STYLE_USAGE ( .BOTH. , #5688 ) ;
#5498 = ADVANCED_FACE ( 'NONE', ( #12443 ), #17074, .F. ) ;
#5499 = ORIENTED_EDGE ( 'NONE', *, *, #18201, .F. ) ;
#5500 = CARTESIAN_POINT ( 'NONE',  ( -34.99999999999998579, 3.000000000000000000, 23.50000000000000711 ) ) ;
#5501 = LINE ( 'NONE', #15961, #13950 ) ;
#5502 = DIRECTION ( 'NONE',  ( 1.000000000000000000, 0.000000000000000000, 0.000000000000000000 ) ) ;
#5503 = EDGE_CURVE ( 'NONE', #11214, #3014, #13800, .T. ) ;
#5504 = ORIENTED_EDGE ( 'NONE', *, *, #11420, .F. ) ;
#5505 = EDGE_CURVE ( 'NONE', #18128, #2161, #10184, .T. ) ;
#5506 =( BOUNDED_SURFACE ( )  B_SPLINE_SURFACE ( 3, 2, ( 
 ( #10326, #19781, #15074 ),
 ( #15277, #1122, #921 ),
 ( #7245, #13527, #4163 ),
 ( #5897, #10435, #9095 ),
 ( #16829, #2587, #7342 ),
 ( #2688, #19588, #19991 ),
 ( #13622, #12088, #10627 ),
 ( #8977, #7457, #8503 ),
 ( #14455, #10195, #13313 ),
 ( #704, #19564, #11257 ),
 ( #19757, #11371, #5091 ),
 ( #19077, #5471, #14838 ) ),
 .UNSPECIFIED., .F., .F., .T. ) 
 B_SPLINE_SURFACE_WITH_KNOTS ( ( 4, 2, 2, 2, 2, 4 ),
 ( 3, 3 ),
 ( 0.001338278704687140058, 0.002129672239503333821, 0.002525369006911430594, 0.002921065774319527367, 0.003712459309135720913, 0.004503852843951914459 ),
 ( 0.000000000000000000, 1.000000000000000000 ),
 .UNSPECIFIED. ) 
 GEOMETRIC_REPRESENTATION_ITEM ( )  RATIONAL_B_SPLINE_SURFACE ( (
 ( 1.000000000000000000, 0.7290225827585891105, 1.000000000000000000),
 ( 1.000000000000000000, 0.7289486400731624016, 1.000000000000000000),
 ( 1.000000000000000000, 0.7309044250879849214, 1.000000000000000000),
 ( 1.000000000000000000, 0.7347910907188455187, 1.000000000000000000),
 ( 1.000000000000000000, 0.7362115201279648691, 1.000000000000000000),
 ( 1.000000000000000000, 0.7387494832161207725, 1.000000000000000000),
 ( 1.000000000000000000, 0.7398605621277711819, 1.000000000000000000),
 ( 1.000000000000000000, 0.7416352795026123212, 1.000000000000000000),
 ( 1.000000000000000000, 0.7406868835584125010, 1.000000000000000000),
 ( 1.000000000000000000, 0.7304426651937115933, 1.000000000000000000),
 ( 1.000000000000000000, 0.7210170799402795261, 1.000000000000000000),
 ( 1.000000000000000000, 0.7071067811865475727, 1.000000000000000000) ) ) 
 REPRESENTATION_ITEM ( '' )  SURFACE ( )  );
#5507 = ORIENTED_EDGE ( 'NONE', *, *, #16689, .F. ) ;
#5508 = FACE_OUTER_BOUND ( 'NONE', #12392, .T. ) ;
#5509 = DIRECTION ( 'NONE',  ( -1.000000000000000000, 0.000000000000000000, 5.551115123125782702E-14 ) ) ;
#5510 = ORIENTED_EDGE ( 'NONE', *, *, #1418, .F. ) ;
#5511 = DIRECTION ( 'NONE',  ( 1.025567617263343161E-15, 0.7071067811865455743, 0.7071067811865493491 ) ) ;
#5512 = DIRECTION ( 'NONE',  ( -1.000000000000000000, 0.000000000000000000, 0.000000000000000000 ) ) ;
#5513 = UNCERTAINTY_MEASURE_WITH_UNIT (LENGTH_MEASURE( 1.000000000000000082E-05 ), #3497, 'distance_accuracy_value', 'NONE');
#5514 = DIRECTION ( 'NONE',  ( 1.000000000000000000, 0.000000000000000000, 0.000000000000000000 ) ) ;
#5515 = DIRECTION ( 'NONE',  ( -1.000000000000000000, 0.000000000000000000, 0.000000000000000000 ) ) ;
#5516 = CARTESIAN_POINT ( 'NONE',  ( -19.00000000000001776, 8.000000000000000000, 40.00000000000000711 ) ) ;
#5517 = STYLED_ITEM ( 'NONE', ( #9254 ), #4004 ) ;
#5518 = ORIENTED_EDGE ( 'NONE', *, *, #7759, .F. ) ;
#5519 = CARTESIAN_POINT ( 'NONE',  ( 0.000000000000000000, 306.0487089519837696, -155.0000000000038369 ) ) ;
#5520 = FACE_OUTER_BOUND ( 'NONE', #18029, .T. ) ;
#5521 = DIRECTION ( 'NONE',  ( 1.000000000000000000, 9.815121534730717399E-17, -0.000000000000000000 ) ) ;
#5522 = SURFACE_STYLE_FILL_AREA ( #8504 ) ;
#5523 = ADVANCED_FACE ( 'NONE', ( #13875 ), #6055, .F. ) ;
#5524 = VERTEX_POINT ( 'NONE', #18156 ) ;
#5525 = VERTEX_POINT ( 'NONE', #1030 ) ;
#5526 = ORIENTED_EDGE ( 'NONE', *, *, #7218, .T. ) ;
#5527 = AXIS2_PLACEMENT_3D ( 'NONE', #5245, #13187, #682 ) ;
#5528 = EDGE_LOOP ( 'NONE', ( #9193, #11605 ) ) ;
#5529 = ORIENTED_EDGE ( 'NONE', *, *, #18808, .T. ) ;
#5530 = PLANE ( 'NONE',  #5142 ) ;
#5531 = DIRECTION ( 'NONE',  ( -0.000000000000000000, -0.000000000000000000, 1.000000000000000000 ) ) ;
#5532 = ORIENTED_EDGE ( 'NONE', *, *, #314, .T. ) ;
#5533 = CARTESIAN_POINT ( 'NONE',  ( 88.88953019741013861, 80.91625508013694912, 245.0000000000000000 ) ) ;
#5534 =( NAMED_UNIT ( * ) PLANE_ANGLE_UNIT ( ) SI_UNIT ( $, .RADIAN. ) );
#5535 = PLANE ( 'NONE',  #6596 ) ;
#5536 = LINE ( 'NONE', #19339, #13890 ) ;
#5537 = CARTESIAN_POINT ( 'NONE',  ( 1.000000000002633893, 138.7723821175183900, 490.5025619656395861 ) ) ;
#5538 = CARTESIAN_POINT ( 'NONE',  ( 32.99999999999998579, 10.00000000000000000, 25.99999999999999645 ) ) ;
#5539 = DIRECTION ( 'NONE',  ( -0.000000000000000000, -1.000000000000000000, -0.000000000000000000 ) ) ;
#5540 = CARTESIAN_POINT ( 'NONE',  ( 1.224646799147349016E-16, 66.00000000000000000, -0.9999999999999972244 ) ) ;
#5541 = PLANE ( 'NONE',  #5134 ) ;
#5542 = FILL_AREA_STYLE ('',( #15029 ) ) ;
#5543 = PRESENTATION_STYLE_ASSIGNMENT (( #7300 ) ) ;
#5544 = AXIS2_PLACEMENT_3D ( 'NONE', #13077, #11399, #567 ) ;
#5545 = FACE_OUTER_BOUND ( 'NONE', #7620, .T. ) ;
#5546 = FACE_OUTER_BOUND ( 'NONE', #18949, .T. ) ;
#5547 = ORIENTED_EDGE ( 'NONE', *, *, #3219, .F. ) ;
#5548 = ORIENTED_EDGE ( 'NONE', *, *, #2175, .T. ) ;
#5549 = UNCERTAINTY_MEASURE_WITH_UNIT (LENGTH_MEASURE( 1.000000000000000082E-05 ), #5019, 'distance_accuracy_value', 'NONE');
#5550 = PRODUCT_DEFINITION_CONTEXT ( 'detailed design', #4593, 'design' ) ;
#5551 = EDGE_LOOP ( 'NONE', ( #11870, #15014, #1951, #1535 ) ) ;
#5552 = EDGE_CURVE ( 'NONE', #2527, #16622, #7358, .T. ) ;
#5553 = VERTEX_POINT ( 'NONE', #12003 ) ;
#5554 = DIRECTION ( 'NONE',  ( 1.000000000000000000, 9.815121534730717399E-17, 0.000000000000000000 ) ) ;
#5555 = COLOUR_RGB ( '', 0.09019608, 0.27058824, 0.51372549) ;
#5556 = SURFACE_STYLE_USAGE ( .BOTH. , #2554 ) ;
#5557 = DIRECTION ( 'NONE',  ( 0.000000000000000000, 0.000000000000000000, -1.000000000000000000 ) ) ;
#5558 = DIRECTION ( 'NONE',  ( 1.000000000000000000, 9.815121534730718631E-17, 0.000000000000000000 ) ) ;
#5559 = LINE ( 'NONE', #18114, #7493 ) ;
#5560 = DIRECTION ( 'NONE',  ( 0.000000000000000000, 0.000000000000000000, 1.000000000000000000 ) ) ;
#5561 = CARTESIAN_POINT ( 'NONE',  ( 498.8117674897343932, 191.8198460455371333, 178.2339398819846110 ) ) ;
#5562 = CARTESIAN_POINT ( 'NONE',  ( -38.50085094405407204, 175.4489062796178871, 505.3921618609452935 ) ) ;
#5563 = CARTESIAN_POINT ( 'NONE',  ( 0.000000000000000000, 219.7545334744432921, 512.1946179577817020 ) ) ;
#5564 = DIRECTION ( 'NONE',  ( 0.000000000000000000, -0.5937146717273790175, -0.8046756418431283420 ) ) ;
#5565 = ADVANCED_FACE ( 'NONE', ( #18363 ), #8805, .F. ) ;
#5566 = CARTESIAN_POINT ( 'NONE',  ( -31.81980515339462912, 0.000000000000000000, 28.51980515339464972 ) ) ;
#5567 = AXIS2_PLACEMENT_3D ( 'NONE', #8785, #19772, #18345 ) ;
#5568 =( GEOMETRIC_REPRESENTATION_CONTEXT ( 3 ) GLOBAL_UNCERTAINTY_ASSIGNED_CONTEXT ( ( #16151 ) ) GLOBAL_UNIT_ASSIGNED_CONTEXT ( ( #8626, #14925, #2136 ) ) REPRESENTATION_CONTEXT ( 'NONE', 'WORKASPACE' ) );
#5569 = COLOUR_RGB ( '', 0.72549020, 0.75294118, 0.79215686) ;
#5570 = ORIENTED_EDGE ( 'NONE', *, *, #5476, .F. ) ;
#5571 = VERTEX_POINT ( 'NONE', #11899 ) ;
#5572 = ORIENTED_EDGE ( 'NONE', *, *, #18786, .F. ) ;
#5573 = ORIENTED_EDGE ( 'NONE', *, *, #8859, .F. ) ;
#5574 = DIRECTION ( 'NONE',  ( -1.000000000000000000, -0.000000000000000000, 0.000000000000000000 ) ) ;
#5575 = EDGE_CURVE ( 'NONE', #4974, #14996, #11846, .T. ) ;
#5576 = DIRECTION ( 'NONE',  ( 0.000000000000000000, 0.000000000000000000, 1.000000000000000000 ) ) ;
#5577 = CARTESIAN_POINT ( 'NONE',  ( -82.18192946989240966, 216.7545334744432921, 489.5655098179820470 ) ) ;
#5578 = CARTESIAN_POINT ( 'NONE',  ( 1.181929469893224560, 139.4861549369088323, 500.2186618848270996 ) ) ;
#5579 = VECTOR ( 'NONE', #7261, 1000.000000000000000 ) ;
#5580 = EDGE_CURVE ( 'NONE', #18077, #1892, #18272, .T. ) ;
#5581 = PLANE ( 'NONE',  #10957 ) ;
#5582 = FILL_AREA_STYLE_COLOUR ( '', #3091 ) ;
#5583 = DIRECTION ( 'NONE',  ( 0.000000000000000000, 0.000000000000000000, -1.000000000000000000 ) ) ;
#5584 = DIRECTION ( 'NONE',  ( -0.000000000000000000, -1.000000000000000000, -0.000000000000000000 ) ) ;
#5585 = CARTESIAN_POINT ( 'NONE',  ( 3.000000000000000000, 1.836909530733570325E-16, 3.000000000000000000 ) ) ;
#5586 = EDGE_LOOP ( 'NONE', ( #2101, #7745, #20103, #10012 ) ) ;
#5587 = PRESENTATION_STYLE_ASSIGNMENT (( #5999 ) ) ;
#5588 = DIRECTION ( 'NONE',  ( 0.000000000000000000, 0.000000000000000000, 1.000000000000000000 ) ) ;
#5589 = CARTESIAN_POINT ( 'NONE',  ( -40.00000000000000000, 68.00000000000000000, -25.99999999999999645 ) ) ;
#5590 = EDGE_CURVE ( 'NONE', #18458, #4219, #3623, .T. ) ;
#5591 = EDGE_CURVE ( 'NONE', #12975, #14376, #2936, .T. ) ;
#5592 = COLOUR_RGB ( '', 0.09019608, 0.27058824, 0.51372549) ;
#5593 = VECTOR ( 'NONE', #10470, 1000.000000000000000 ) ;
#5594 = PRESENTATION_LAYER_ASSIGNMENT (  '', '', ( #13818 ) ) ;
#5595 = EDGE_LOOP ( 'NONE', ( #19142, #13199, #8896, #11507 ) ) ;
#5596 = ORIENTED_EDGE ( 'NONE', *, *, #14940, .F. ) ;
#5597 = EDGE_CURVE ( 'NONE', #16250, #19193, #6255, .T. ) ;
#5598 = EDGE_LOOP ( 'NONE', ( #17173, #18479, #4847, #10920 ) ) ;
#5599 = DIRECTION ( 'NONE',  ( 0.000000000000000000, 1.000000000000000000, 0.000000000000000000 ) ) ;
#5600 = UNCERTAINTY_MEASURE_WITH_UNIT (LENGTH_MEASURE( 1.000000000000000082E-05 ), #12950, 'distance_accuracy_value', 'NONE');
#5601 = ORIENTED_EDGE ( 'NONE', *, *, #12673, .T. ) ;
#5602 =( NAMED_UNIT ( * ) PLANE_ANGLE_UNIT ( ) SI_UNIT ( $, .RADIAN. ) );
#5603 = CARTESIAN_POINT ( 'NONE',  ( 53.48937290013659407, 145.9162550801369491, 0.000000000000000000 ) ) ;
#5604 = CARTESIAN_POINT ( 'NONE',  ( -20.00000000000003197, 0.000000000000000000, 40.00000000000000711 ) ) ;
#5605 = LINE ( 'NONE', #15398, #5443 ) ;
#5606 = VECTOR ( 'NONE', #19758, 1000.000000000000000 ) ;
#5607 = LINE ( 'NONE', #7071, #12027 ) ;
#5608 = EDGE_CURVE ( 'NONE', #5100, #7117, #19693, .T. ) ;
#5609 = AXIS2_PLACEMENT_3D ( 'NONE', #17267, #20342, #18793 ) ;
#5610 = LINE ( 'NONE', #7072, #4584 ) ;
#5611 = VECTOR ( 'NONE', #2179, 1000.000000000000000 ) ;
#5612 = STYLED_ITEM ( 'NONE', ( #5680 ), #6193 ) ;
#5613 = SURFACE_STYLE_USAGE ( .BOTH. , #4272 ) ;
#5614 = VERTEX_POINT ( 'NONE', #11701 ) ;
#5615 =( NAMED_UNIT ( * ) PLANE_ANGLE_UNIT ( ) SI_UNIT ( $, .RADIAN. ) );
#5616 =( LENGTH_UNIT ( ) NAMED_UNIT ( * ) SI_UNIT ( .MILLI., .METRE. ) );
#5617 = SURFACE_STYLE_USAGE ( .BOTH. , #20120 ) ;
#5618 = APPLICATION_PROTOCOL_DEFINITION ( 'draft international standard', 'automotive_design', 1998, #13432 ) ;
#5619 = ADVANCED_FACE ( 'NONE', ( #7170 ), #8897, .F. ) ;
#5620 = ORIENTED_EDGE ( 'NONE', *, *, #2690, .T. ) ;
#5621 =( NAMED_UNIT ( * ) SI_UNIT ( $, .STERADIAN. ) SOLID_ANGLE_UNIT ( ) );
#5622 = VECTOR ( 'NONE', #4016, 1000.000000000000000 ) ;
#5623 = EDGE_CURVE ( 'NONE', #11912, #8401, #8585, .T. ) ;
#5624 = ORIENTED_EDGE ( 'NONE', *, *, #2609, .T. ) ;
#5625 = ORIENTED_EDGE ( 'NONE', *, *, #15759, .T. ) ;
#5626 = EDGE_LOOP ( 'NONE', ( #3558, #5789, #5056, #614 ) ) ;
#5627 = AXIS2_PLACEMENT_3D ( 'NONE', #529, #16421, #718 ) ;
#5628 = DIRECTION ( 'NONE',  ( 1.000000000000000000, 0.000000000000000000, 0.000000000000000000 ) ) ;
#5629 = VERTEX_POINT ( 'NONE', #7068 ) ;
#5630 = SURFACE_STYLE_FILL_AREA ( #19717 ) ;
#5631 = DIRECTION ( 'NONE',  ( 0.000000000000000000, -0.3129478523439812032, 0.9497703099767278445 ) ) ;
#5632 = VERTEX_POINT ( 'NONE', #14775 ) ;
#5633 = LINE ( 'NONE', #16975, #8063 ) ;
#5634 = DIRECTION ( 'NONE',  ( 0.000000000000000000, 1.000000000000000000, 0.000000000000000000 ) ) ;
#5635 = DIRECTION ( 'NONE',  ( 1.000000000000000000, 0.000000000000000000, 0.000000000000000000 ) ) ;
#5636 = PRESENTATION_STYLE_ASSIGNMENT (( #15118 ) ) ;
#5637 = CARTESIAN_POINT ( 'NONE',  ( 21.99999999999998224, 8.000000000000000000, -35.99999999999999289 ) ) ;
#5638 = ADVANCED_FACE ( 'NONE', ( #13363, #10237 ), #13541, .F. ) ;
#5639 = DIRECTION ( 'NONE',  ( -8.027491443112700323E-16, -0.7071067811865504593, 0.7071067811865445751 ) ) ;
#5640 =( GEOMETRIC_REPRESENTATION_CONTEXT ( 3 ) GLOBAL_UNCERTAINTY_ASSIGNED_CONTEXT ( ( #2679 ) ) GLOBAL_UNIT_ASSIGNED_CONTEXT ( ( #20149, #18503, #10689 ) ) REPRESENTATION_CONTEXT ( 'NONE', 'WORKASPACE' ) );
#5641 = LINE ( 'NONE', #880, #10635 ) ;
#5642 = CARTESIAN_POINT ( 'NONE',  ( -44.50085094405407915, 175.4489062796178871, 505.3921618609452935 ) ) ;
#5643 = VECTOR ( 'NONE', #12899, 1000.000000000000000 ) ;
#5644 = DIRECTION ( 'NONE',  ( 0.000000000000000000, -0.000000000000000000, 1.000000000000000000 ) ) ;
#5645 = SURFACE_STYLE_USAGE ( .BOTH. , #15031 ) ;
#5646 = CARTESIAN_POINT ( 'NONE',  ( 18.99999999999998224, 8.000000000000000000, -39.99999999999999289 ) ) ;
#5647 = EDGE_LOOP ( 'NONE', ( #15209, #9934, #1907, #7459 ) ) ;
#5648 = ADVANCED_FACE ( 'NONE', ( #2604 ), #16542, .F. ) ;
#5649 = ORIENTED_EDGE ( 'NONE', *, *, #18040, .T. ) ;
#5650 = VERTEX_POINT ( 'NONE', #13456 ) ;
#5651 = ORIENTED_EDGE ( 'NONE', *, *, #18438, .T. ) ;
#5652 = CARTESIAN_POINT ( 'NONE',  ( -211.5106270998635409, 123.1299228374912644, 29.36128450348865471 ) ) ;
#5653 = AXIS2_PLACEMENT_3D ( 'NONE', #12131, #1266, #2849 ) ;
#5654 = CYLINDRICAL_SURFACE ( 'NONE', #11002, 4.999999999999997335 ) ;
#5655 = CARTESIAN_POINT ( 'NONE',  ( 111.4893729001366012, 122.8810204491430369, 322.0399576098686225 ) ) ;
#5656 = STYLED_ITEM ( 'NONE', ( #19330 ), #8670 ) ;
#5657 = CARTESIAN_POINT ( 'NONE',  ( 0.000000000000000000, 341.0487089519837696, -96.50000000000331113 ) ) ;
#5658 = LINE ( 'NONE', #10597, #7031 ) ;
#5659 = LINE ( 'NONE', #17821, #5844 ) ;
#5660 = DIRECTION ( 'NONE',  ( 1.000000000000000000, 0.000000000000000000, -0.000000000000000000 ) ) ;
#5661 = LINE ( 'NONE', #11960, #17117 ) ;
#5662 = DIRECTION ( 'NONE',  ( 0.000000000000000000, -0.000000000000000000, -1.000000000000000000 ) ) ;
#5663 = EDGE_CURVE ( 'NONE', #3506, #11785, #16366, .T. ) ;
#5664 = FACE_OUTER_BOUND ( 'NONE', #5117, .T. ) ;
#5665 = SURFACE_STYLE_FILL_AREA ( #13897 ) ;
#5666 = DIRECTION ( 'NONE',  ( 0.000000000000000000, -1.000000000000000000, 0.000000000000000000 ) ) ;
#5667 = COLOUR_RGB ( '', 0.09019608, 0.27058824, 0.51372549) ;
#5668 = VECTOR ( 'NONE', #12873, 1000.000000000000000 ) ;
#5669 = ORIENTED_EDGE ( 'NONE', *, *, #1834, .F. ) ;
#5670 = ORIENTED_EDGE ( 'NONE', *, *, #19801, .T. ) ;
#5671 = COLOUR_RGB ( '', 0.66274510, 0.83137255, 0.94901961) ;
#5672 = FACE_BOUND ( 'NONE', #11610, .T. ) ;
#5673 = ORIENTED_EDGE ( 'NONE', *, *, #1180, .T. ) ;
#5674 = ORIENTED_EDGE ( 'NONE', *, *, #3244, .T. ) ;
#5675 = ORIENTED_EDGE ( 'NONE', *, *, #17826, .T. ) ;
#5676 = LINE ( 'NONE', #4338, #3675 ) ;
#5677 = COLOUR_RGB ( '', 0.66274510, 0.83137255, 0.94901961) ;
#5678 = CIRCLE ( 'NONE', #3372, 8.000000000000000000 ) ;
#5679 = AXIS2_PLACEMENT_3D ( 'NONE', #13870, #1685, #1260 ) ;
#5680 = PRESENTATION_STYLE_ASSIGNMENT (( #2579 ) ) ;
#5681 = DIRECTION ( 'NONE',  ( -0.000000000000000000, -1.000000000000000000, -0.000000000000000000 ) ) ;
#5682 = CARTESIAN_POINT ( 'NONE',  ( 35.00000000000000711, 19.00000000000000000, 20.99999999999999289 ) ) ;
#5683 = CARTESIAN_POINT ( 'NONE',  ( 32.99999999999998579, 8.000000000000000000, 21.99999999999999645 ) ) ;
#5684 = PRESENTATION_LAYER_ASSIGNMENT (  '', '', ( #5373 ) ) ;
#5685 = DIRECTION ( 'NONE',  ( 0.000000000000000000, 0.000000000000000000, 1.000000000000000000 ) ) ;
#5686 = LINE ( 'NONE', #8878, #18178 ) ;
#5687 = CARTESIAN_POINT ( 'NONE',  ( -79.99999999999995737, 316.7545334744432353, 515.1946179577817020 ) ) ;
#5688 = SURFACE_SIDE_STYLE ('',( #10220 ) ) ;
#5689 = VECTOR ( 'NONE', #14269, 1000.000000000000000 ) ;
#5690 = ORIENTED_EDGE ( 'NONE', *, *, #17964, .T. ) ;
#5691 = DIRECTION ( 'NONE',  ( -1.000000000000000000, 0.000000000000000000, -0.000000000000000000 ) ) ;
#5692 = VECTOR ( 'NONE', #4865, 1000.000000000000000 ) ;
#5693 = DIRECTION ( 'NONE',  ( -1.000000000000000000, 0.000000000000000000, 0.000000000000000000 ) ) ;
#5694 = DIRECTION ( 'NONE',  ( 0.000000000000000000, -1.000000000000000000, 0.000000000000000000 ) ) ;
#5695 = EDGE_CURVE ( 'NONE', #16024, #10866, #3462, .T. ) ;
#5696 = CIRCLE ( 'NONE', #2051, 0.9999999999999964473 ) ;
#5697 = CIRCLE ( 'NONE', #17212, 5.000000000000004441 ) ;
#5698 = PRODUCT_DEFINITION ( 'UNKNOWN', '', #411, #14817 ) ;
#5699 = EDGE_LOOP ( 'NONE', ( #7510, #17833, #15708, #8867 ) ) ;
#5700 = EDGE_LOOP ( 'NONE', ( #20290, #3290, #8316, #11743 ) ) ;
#5701 = EDGE_CURVE ( 'NONE', #2573, #10931, #8409, .T. ) ;
#5702 = FACE_OUTER_BOUND ( 'NONE', #4541, .T. ) ;
#5703 = DIRECTION ( 'NONE',  ( 0.000000000000000000, 1.000000000000000000, 0.000000000000000000 ) ) ;
#5704 = ORIENTED_EDGE ( 'NONE', *, *, #4709, .F. ) ;
#5705 = DIRECTION ( 'NONE',  ( -1.000000000000000000, 0.000000000000000000, 0.000000000000000000 ) ) ;
#5706 =( NAMED_UNIT ( * ) SI_UNIT ( $, .STERADIAN. ) SOLID_ANGLE_UNIT ( ) );
#5707 = SURFACE_SIDE_STYLE ('',( #7263 ) ) ;
#5708 = CIRCLE ( 'NONE', #2401, 4.999999999999997335 ) ;
#5709 = AXIS2_PLACEMENT_3D ( 'NONE', #7479, #12198, #11910 ) ;
#5710 = CARTESIAN_POINT ( 'NONE',  ( -80.58226053856785143, 140.4824639777437199, 500.9116485922544371 ) ) ;
#5711 = ORIENTED_EDGE ( 'NONE', *, *, #13666, .T. ) ;
#5712 = CARTESIAN_POINT ( 'NONE',  ( -31.00000000000007105, 10.00000000000000000, 23.00000000000000000 ) ) ;
#5713 = CARTESIAN_POINT ( 'NONE',  ( 82.88953019741013861, 167.9162550801369491, 245.0000000000000000 ) ) ;
#5714 = PRESENTATION_STYLE_ASSIGNMENT (( #5617 ) ) ;
#5715 = SHAPE_DEFINITION_REPRESENTATION ( #10731, #13798 ) ;
#5716 = EDGE_CURVE ( 'NONE', #16910, #14575, #10051, .T. ) ;
#5717 = PRESENTATION_LAYER_ASSIGNMENT (  '', '', ( #14602 ) ) ;
#5718 = EDGE_CURVE ( 'NONE', #4612, #10163, #17767, .T. ) ;
#5719 = VERTEX_POINT ( 'NONE', #742 ) ;
#5720 = ORIENTED_EDGE ( 'NONE', *, *, #14282, .T. ) ;
#5721 = AXIS2_PLACEMENT_3D ( 'NONE', #19096, #247, #6549 ) ;
#5722 =( GEOMETRIC_REPRESENTATION_CONTEXT ( 3 ) GLOBAL_UNCERTAINTY_ASSIGNED_CONTEXT ( ( #16700 ) ) GLOBAL_UNIT_ASSIGNED_CONTEXT ( ( #11287, #14082, #10888 ) ) REPRESENTATION_CONTEXT ( 'NONE', 'WORKASPACE' ) );
#5723 = ORIENTED_EDGE ( 'NONE', *, *, #6477, .T. ) ;
#5724 = ORIENTED_EDGE ( 'NONE', *, *, #3718, .F. ) ;
#5725 = EDGE_CURVE ( 'NONE', #2779, #584, #11512, .T. ) ;
#5726 = ORIENTED_EDGE ( 'NONE', *, *, #5597, .F. ) ;
#5727 = COLOUR_RGB ( '', 0.72549020, 0.75294118, 0.79215686) ;
#5728 = AXIS2_PLACEMENT_3D ( 'NONE', #17961, #6761, #10037 ) ;
#5729 = PRESENTATION_LAYER_ASSIGNMENT (  '', '', ( #17950 ) ) ;
#5730 = STYLED_ITEM ( 'NONE', ( #2462 ), #8010 ) ;
#5731 = ADVANCED_FACE ( 'NONE', ( #19601 ), #14574, .T. ) ;
#5732 = FACE_OUTER_BOUND ( 'NONE', #18781, .T. ) ;
#5733 = EDGE_LOOP ( 'NONE', ( #3222, #13031 ) ) ;
#5734 = LINE ( 'NONE', #3348, #7431 ) ;
#5735 = CARTESIAN_POINT ( 'NONE',  ( 0.000000000000000000, 313.8311070602663904, -87.78239810828596035 ) ) ;
#5736 = ORIENTED_EDGE ( 'NONE', *, *, #12574, .F. ) ;
#5737 = CARTESIAN_POINT ( 'NONE',  ( 78.48937290013660117, 113.1299228374914208, 79.58252780074349175 ) ) ;
#5738 = VECTOR ( 'NONE', #11152, 1000.000000000000000 ) ;
#5739 = DIRECTION ( 'NONE',  ( -0.000000000000000000, -1.000000000000000000, -0.000000000000000000 ) ) ;
#5740 = VECTOR ( 'NONE', #18633, 1000.000000000000227 ) ;
#5741 = EDGE_CURVE ( 'NONE', #2973, #7546, #19094, .T. ) ;
#5742 = CARTESIAN_POINT ( 'NONE',  ( 10.00000000000000000, 301.0487089519837127, -150.0000000000038369 ) ) ;
#5743 = DIRECTION ( 'NONE',  ( 0.000000000000000000, 0.000000000000000000, -1.000000000000000000 ) ) ;
#5744 = DIRECTION ( 'NONE',  ( 0.000000000000000000, 0.000000000000000000, 1.000000000000000000 ) ) ;
#5745 = DIRECTION ( 'NONE',  ( -1.000000000000000000, -0.000000000000000000, -0.000000000000000000 ) ) ;
#5746 = CARTESIAN_POINT ( 'NONE',  ( 31.00000000000003553, 19.00000000000000000, 20.99999999999999289 ) ) ;
#5747 = PRESENTATION_LAYER_ASSIGNMENT (  '', '', ( #4101 ) ) ;
#5748 = AXIS2_PLACEMENT_3D ( 'NONE', #109, #7847, #14127 ) ;
#5749 = CARTESIAN_POINT ( 'NONE',  ( 40.00000000000001421, 3.000000000000000888, 0.000000000000000000 ) ) ;
#5750 = DIRECTION ( 'NONE',  ( 0.000000000000000000, -1.000000000000000000, 0.000000000000000000 ) ) ;
#5752 =( GEOMETRIC_REPRESENTATION_CONTEXT ( 3 ) GLOBAL_UNCERTAINTY_ASSIGNED_CONTEXT ( ( #5185 ) ) GLOBAL_UNIT_ASSIGNED_CONTEXT ( ( #6722, #8359, #16019 ) ) REPRESENTATION_CONTEXT ( 'NONE', 'WORKASPACE' ) );
#5751 = FILL_AREA_STYLE ('',( #19838 ) ) ;
#5753 = PLANE ( 'NONE',  #11596 ) ;
#5754 = CIRCLE ( 'NONE', #5092, 7.999999999999996447 ) ;
#5755 = DIRECTION ( 'NONE',  ( 0.000000000000000000, 1.000000000000000000, 0.000000000000000000 ) ) ;
#5756 = EDGE_CURVE ( 'NONE', #13105, #16250, #11483, .T. ) ;
#5757 = ORIENTED_EDGE ( 'NONE', *, *, #11793, .F. ) ;
#5758 = LINE ( 'NONE', #4397, #16215 ) ;
#5759 = CARTESIAN_POINT ( 'NONE',  ( 37.00000000000003553, 3.000000000000000000, 20.00000000000000000 ) ) ;
#5760 = ORIENTED_EDGE ( 'NONE', *, *, #20332, .F. ) ;
#5761 = AXIS2_PLACEMENT_3D ( 'NONE', #13387, #17696, #12976 ) ;
#5762 = DIRECTION ( 'NONE',  ( 0.000000000000000000, 0.000000000000000000, -1.000000000000000000 ) ) ;
#5763 = ORIENTED_EDGE ( 'NONE', *, *, #15301, .F. ) ;
#5764 = UNCERTAINTY_MEASURE_WITH_UNIT (LENGTH_MEASURE( 1.000000000000000082E-05 ), #17375, 'distance_accuracy_value', 'NONE');
#5765 = VERTEX_POINT ( 'NONE', #16153 ) ;
#5766 = ORIENTED_EDGE ( 'NONE', *, *, #10125, .T. ) ;
#5767 = EDGE_CURVE ( 'NONE', #15368, #20073, #19123, .T. ) ;
#5768 = VECTOR ( 'NONE', #13371, 1000.000000000000000 ) ;
#5769 = CARTESIAN_POINT ( 'NONE',  ( -79.22030824640687285, 138.9228415808856596, 489.3162532734729098 ) ) ;
#5770 = AXIS2_PLACEMENT_3D ( 'NONE', #12816, #6130, #4665 ) ;
#5771 = DIRECTION ( 'NONE',  ( -1.000000000000000000, -0.000000000000000000, -1.135258727068399668E-15 ) ) ;
#5772 = CARTESIAN_POINT ( 'NONE',  ( -25.99999999999999645, 68.00000000000000000, 40.00000000000002132 ) ) ;
#5773 = CIRCLE ( 'NONE', #6434, 10.00000000000000888 ) ;
#5774 = CARTESIAN_POINT ( 'NONE',  ( -37.00000000000000711, 6.000000000000000000, -23.00000000000000000 ) ) ;
#5775 = CARTESIAN_POINT ( 'NONE',  ( -26.00000000000000355, 19.00000000000000000, 31.00000000000003197 ) ) ;
#5776 = EDGE_CURVE ( 'NONE', #2425, #6883, #19495, .T. ) ;
#5777 = CARTESIAN_POINT ( 'NONE',  ( 3.000000000000000000, 1.836909530733565148E-16, 22.00000000000000000 ) ) ;
#5778 = COLOUR_RGB ( '', 0.66274510, 0.83137255, 0.94901961) ;
#5779 = CARTESIAN_POINT ( 'NONE',  ( 4.469960816887838430E-15, 3.000000000000000000, 36.50000000000000000 ) ) ;
#5780 = MECHANICAL_DESIGN_GEOMETRIC_PRESENTATION_REPRESENTATION (  '', ( #18919 ), #3079 ) ;
#5781 = SURFACE_STYLE_FILL_AREA ( #2765 ) ;
#5782 = CARTESIAN_POINT ( 'NONE',  ( 40.00000000000001421, 3.000000000000000888, -150.0000000000000000 ) ) ;
#5783 = DIRECTION ( 'NONE',  ( -0.000000000000000000, -0.000000000000000000, 1.000000000000000000 ) ) ;
#5784 =( LENGTH_UNIT ( ) NAMED_UNIT ( * ) SI_UNIT ( .MILLI., .METRE. ) );
#5785 = DIRECTION ( 'NONE',  ( 0.000000000000000000, 0.000000000000000000, -1.000000000000000000 ) ) ;
#5786 = AXIS2_PLACEMENT_3D ( 'NONE', #8564, #17847, #19586 ) ;
#5787 = ADVANCED_FACE ( 'NONE', ( #17971 ), #3863, .F. ) ;
#5788 = ORIENTED_EDGE ( 'NONE', *, *, #15909, .F. ) ;
#5789 = ORIENTED_EDGE ( 'NONE', *, *, #18132, .F. ) ;
#5790 = AXIS2_PLACEMENT_3D ( 'NONE', #15396, #4468, #15612 ) ;
#5791 = ORIENTED_EDGE ( 'NONE', *, *, #19579, .F. ) ;
#5792 = ORIENTED_EDGE ( 'NONE', *, *, #13370, .F. ) ;
#5793 = DIRECTION ( 'NONE',  ( 0.000000000000000000, 1.000000000000000000, 0.000000000000000000 ) ) ;
#5794 = DIRECTION ( 'NONE',  ( -0.000000000000000000, 0.000000000000000000, -1.000000000000000000 ) ) ;
#5795 = UNCERTAINTY_MEASURE_WITH_UNIT (LENGTH_MEASURE( 1.000000000000000082E-05 ), #17140, 'distance_accuracy_value', 'NONE');
#5796 = DIRECTION ( 'NONE',  ( 0.000000000000000000, 0.000000000000000000, 1.000000000000000000 ) ) ;
#5797 =( NAMED_UNIT ( * ) PLANE_ANGLE_UNIT ( ) SI_UNIT ( $, .RADIAN. ) );
#5798 = CARTESIAN_POINT ( 'NONE',  ( 10.00000000000000000, 376.0487089519832011, -80.00000000000332534 ) ) ;
#5799 = DIRECTION ( 'NONE',  ( -1.000000000000000000, 0.000000000000000000, 1.450371633464475582E-15 ) ) ;
#5800 = CARTESIAN_POINT ( 'NONE',  ( 0.000000000000000000, 10.00000000000000000, -9.500000000000000000 ) ) ;
#5801 = CARTESIAN_POINT ( 'NONE',  ( 35.99999999999999289, 8.000000000000000000, 18.99999999999999289 ) ) ;
#5802 = CARTESIAN_POINT ( 'NONE',  ( 0.000000000000000000, 147.7545334744432921, 491.0690926367356042 ) ) ;
#5803 = DIRECTION ( 'NONE',  ( -0.000000000000000000, -1.000000000000000000, -0.000000000000000000 ) ) ;
#5804 = VECTOR ( 'NONE', #3519, 1000.000000000000000 ) ;
#5805 = DIRECTION ( 'NONE',  ( 0.000000000000000000, 0.000000000000000000, 1.000000000000000000 ) ) ;
#5806 = LINE ( 'NONE', #15774, #15215 ) ;
#5807 = ORIENTED_EDGE ( 'NONE', *, *, #115, .T. ) ;
#5808 = SURFACE_STYLE_FILL_AREA ( #15174 ) ;
#5809 = FILL_AREA_STYLE ('',( #13445 ) ) ;
#5810 =( GEOMETRIC_REPRESENTATION_CONTEXT ( 3 ) GLOBAL_UNCERTAINTY_ASSIGNED_CONTEXT ( ( #16006 ) ) GLOBAL_UNIT_ASSIGNED_CONTEXT ( ( #18745, #4334, #15372 ) ) REPRESENTATION_CONTEXT ( 'NONE', 'WORKASPACE' ) );
#5811 = ORIENTED_EDGE ( 'NONE', *, *, #12073, .T. ) ;
#5812 = UNCERTAINTY_MEASURE_WITH_UNIT (LENGTH_MEASURE( 1.000000000000000082E-05 ), #4128, 'distance_accuracy_value', 'NONE');
#5813 = COLOUR_RGB ( '', 0.08235294, 0.09019608, 0.10196078) ;
#5814 = EDGE_CURVE ( 'NONE', #17668, #12426, #12850, .T. ) ;
#5815 = EDGE_LOOP ( 'NONE', ( #9706, #11632, #17913, #4151 ) ) ;
#5816 = LINE ( 'NONE', #9711, #10358 ) ;
#5817 = FACE_BOUND ( 'NONE', #9736, .T. ) ;
#5818 = UNCERTAINTY_MEASURE_WITH_UNIT (LENGTH_MEASURE( 1.000000000000000082E-05 ), #7450, 'distance_accuracy_value', 'NONE');
#5819 = AXIS2_PLACEMENT_3D ( 'NONE', #15666, #12233, #4309 ) ;
#5820 = ORIENTED_EDGE ( 'NONE', *, *, #5701, .T. ) ;
#5821 = CARTESIAN_POINT ( 'NONE',  ( 31.00000000000001421, 10.00000000000000000, 25.99999999999999645 ) ) ;
#5822 = CARTESIAN_POINT ( 'NONE',  ( 503.8334540492693918, 191.8198460455371333, 178.2339398819846110 ) ) ;
#5823 = PRESENTATION_STYLE_ASSIGNMENT (( #10750 ) ) ;
#5824 = CARTESIAN_POINT ( 'NONE',  ( -21.85283368562565443, 319.7545334744432353, 485.1700099148404774 ) ) ;
#5825 = FACE_OUTER_BOUND ( 'NONE', #1519, .T. ) ;
#5826 = PRESENTATION_STYLE_ASSIGNMENT (( #5613 ) ) ;
#5827 = VERTEX_POINT ( 'NONE', #20000 ) ;
#5828 = CARTESIAN_POINT ( 'NONE',  ( 0.000000000000000000, 313.8311070602663904, -142.2176018917206761 ) ) ;
#5829 = CARTESIAN_POINT ( 'NONE',  ( -78.99999999999995737, 152.4824555358011082, 486.3411705753778165 ) ) ;
#5830 = PRODUCT_CONTEXT ( 'NONE', #2487, 'mechanical' ) ;
#5831 = VERTEX_POINT ( 'NONE', #18057 ) ;
#5832 = FILL_AREA_STYLE ('',( #2412 ) ) ;
#5833 = EDGE_CURVE ( 'NONE', #13589, #8514, #319, .T. ) ;
#5834 = VERTEX_POINT ( 'NONE', #15085 ) ;
#5835 = VERTEX_POINT ( 'NONE', #8994 ) ;
#5836 = ORIENTED_EDGE ( 'NONE', *, *, #10758, .F. ) ;
#5837 = CARTESIAN_POINT ( 'NONE',  ( -79.99999999999995737, 316.7545334744432353, 495.1946179577816451 ) ) ;
#5838 = ORIENTED_EDGE ( 'NONE', *, *, #4379, .T. ) ;
#5839 = DIRECTION ( 'NONE',  ( -1.132388935707081510E-15, 0.000000000000000000, 1.000000000000000000 ) ) ;
#5840 = ORIENTED_EDGE ( 'NONE', *, *, #3187, .F. ) ;
#5841 = FILL_AREA_STYLE_COLOUR ( '', #14968 ) ;
#5842 = ADVANCED_FACE ( 'NONE', ( #13834 ), #7168, .F. ) ;
#5843 = PRESENTATION_STYLE_ASSIGNMENT (( #2428 ) ) ;
#5844 = VECTOR ( 'NONE', #4013, 1000.000000000000000 ) ;
#5845 = CARTESIAN_POINT ( 'NONE',  ( -31.00000000000003553, 11.00000000000000000, -26.00000000000000355 ) ) ;
#5846 = CARTESIAN_POINT ( 'NONE',  ( 503.8334540492693918, 191.8198460455371333, 24.99421986894476078 ) ) ;
#5847 = DIRECTION ( 'NONE',  ( -0.003530072958128175308, 0.9999937692730440641, 0.000000000000000000 ) ) ;
#5848 = EDGE_CURVE ( 'NONE', #11820, #4266, #17774, .T. ) ;
#5849 = CARTESIAN_POINT ( 'NONE',  ( 0.000000000000000000, 146.1184945051222428, 479.9772095446988374 ) ) ;
#5850 = PLANE ( 'NONE',  #12941 ) ;
#5851 = CARTESIAN_POINT ( 'NONE',  ( 31.00000000000002842, 68.00000000000000000, 26.00000000000001066 ) ) ;
#5852 = CARTESIAN_POINT ( 'NONE',  ( 30.90550859392620353, 22.88608451763353457, 66.87703344121219118 ) ) ;
#5853 = DIRECTION ( 'NONE',  ( 0.000000000000000000, 1.000000000000000000, 0.000000000000000000 ) ) ;
#5854 = CARTESIAN_POINT ( 'NONE',  ( 31.00000000000003553, 19.00000000000000000, 20.99999999999999289 ) ) ;
#5855 = DIRECTION ( 'NONE',  ( 1.000000000000000000, -0.000000000000000000, -0.000000000000000000 ) ) ;
#5856 =( GEOMETRIC_REPRESENTATION_CONTEXT ( 3 ) GLOBAL_UNCERTAINTY_ASSIGNED_CONTEXT ( ( #11031 ) ) GLOBAL_UNIT_ASSIGNED_CONTEXT ( ( #4271, #7474, #13744 ) ) REPRESENTATION_CONTEXT ( 'NONE', 'WORKASPACE' ) );
#5857 = ORIENTED_EDGE ( 'NONE', *, *, #5329, .T. ) ;
#5858 = EDGE_CURVE ( 'NONE', #9269, #3677, #13453, .T. ) ;
#5859 = AXIS2_PLACEMENT_3D ( 'NONE', #6995, #14920, #14810 ) ;
#5860 = ADVANCED_FACE ( 'NONE', ( #5909 ), #935, .F. ) ;
#5861 = ORIENTED_EDGE ( 'NONE', *, *, #8169, .F. ) ;
#5862 = ORIENTED_EDGE ( 'NONE', *, *, #10742, .T. ) ;
#5863 = ORIENTED_EDGE ( 'NONE', *, *, #2817, .T. ) ;
#5864 = CARTESIAN_POINT ( 'NONE',  ( -79.94176149790892794, 138.7993301623293121, 490.1678215211853740 ) ) ;
#5865 = VERTEX_POINT ( 'NONE', #8894 ) ;
#5866 = CARTESIAN_POINT ( 'NONE',  ( 0.000000000000000000, 372.8685141053783241, -146.8198051533979935 ) ) ;
#5867 = ADVANCED_FACE ( 'NONE', ( #15394 ), #19691, .T. ) ;
#5868 = LINE ( 'NONE', #2760, #10334 ) ;
#5869 = ORIENTED_EDGE ( 'NONE', *, *, #10895, .T. ) ;
#5870 = DIRECTION ( 'NONE',  ( -0.000000000000000000, -1.000000000000000000, -0.000000000000000000 ) ) ;
#5871 = DIRECTION ( 'NONE',  ( -1.000000000000000000, -0.000000000000000000, -0.000000000000000000 ) ) ;
#5872 = FILL_AREA_STYLE ('',( #10296 ) ) ;
#5873 = AXIS2_PLACEMENT_3D ( 'NONE', #12330, #1362, #18708 ) ;
#5874 =( NAMED_UNIT ( * ) SI_UNIT ( $, .STERADIAN. ) SOLID_ANGLE_UNIT ( ) );
#5875 = FILL_AREA_STYLE ('',( #6187 ) ) ;
#5876 = DIRECTION ( 'NONE',  ( 1.000000000000000000, 5.889072920838430686E-16, -0.000000000000000000 ) ) ;
#5877 = FACE_OUTER_BOUND ( 'NONE', #5214, .T. ) ;
#5878 = EDGE_CURVE ( 'NONE', #5238, #12661, #18754, .T. ) ;
#5879 = DIRECTION ( 'NONE',  ( 0.000000000000000000, 0.000000000000000000, -1.000000000000000000 ) ) ;
#5880 = CARTESIAN_POINT ( 'NONE',  ( 31.00000000000000000, 8.000000000000000000, 30.99999999999999289 ) ) ;
#5881 = SURFACE_SIDE_STYLE ('',( #5665 ) ) ;
#5882 = ORIENTED_EDGE ( 'NONE', *, *, #11008, .F. ) ;
#5883 = ORIENTED_EDGE ( 'NONE', *, *, #10136, .T. ) ;
#5884 = AXIS2_PLACEMENT_3D ( 'NONE', #7778, #12507, #236 ) ;
#5885 = ORIENTED_EDGE ( 'NONE', *, *, #17605, .T. ) ;
#5886 = ORIENTED_EDGE ( 'NONE', *, *, #15648, .F. ) ;
#5887 = SURFACE_STYLE_USAGE ( .BOTH. , #15695 ) ;
#5888 = DIRECTION ( 'NONE',  ( 0.000000000000000000, -1.000000000000000000, 0.000000000000000000 ) ) ;
#5889 = CARTESIAN_POINT ( 'NONE',  ( 21.00000000000000000, 19.00000000000000000, 35.00000000000001421 ) ) ;
#5890 = CARTESIAN_POINT ( 'NONE',  ( -31.00000000000003553, 8.000000000000000000, -21.00000000000000000 ) ) ;
#5891 = SURFACE_SIDE_STYLE ('',( #15162 ) ) ;
#5892 = DIRECTION ( 'NONE',  ( -1.000000000000000000, -0.000000000000000000, -0.000000000000000000 ) ) ;
#5893 = EDGE_CURVE ( 'NONE', #8326, #9383, #16656, .T. ) ;
#5894 = CARTESIAN_POINT ( 'NONE',  ( 0.000000000000000000, 306.0487089519837127, -150.0000000000038369 ) ) ;
#5895 = PLANE ( 'NONE',  #12313 ) ;
#5896 = FACE_OUTER_BOUND ( 'NONE', #18784, .T. ) ;
#5897 = CARTESIAN_POINT ( 'NONE',  ( -80.55146305734733403, 139.7860373442720743, 489.4617291895204971 ) ) ;
#5898 = VECTOR ( 'NONE', #17488, 1000.000000000000000 ) ;
#5899 = VERTEX_POINT ( 'NONE', #4059 ) ;
#5900 = FACE_OUTER_BOUND ( 'NONE', #2728, .T. ) ;
#5901 = SURFACE_STYLE_FILL_AREA ( #17115 ) ;
#5902 = EDGE_CURVE ( 'NONE', #716, #16512, #16751, .T. ) ;
#5903 = PLANE ( 'NONE',  #10027 ) ;
#5904 = ORIENTED_EDGE ( 'NONE', *, *, #15710, .T. ) ;
#5905 = STYLED_ITEM ( 'NONE', ( #9371 ), #16097 ) ;
#5906 = AXIS2_PLACEMENT_3D ( 'NONE', #12145, #4621, #20056 ) ;
#5907 = VERTEX_POINT ( 'NONE', #7356 ) ;
#5908 = CARTESIAN_POINT ( 'NONE',  ( 53.48937290013659407, 125.7247684487574588, 252.0000000000000000 ) ) ;
#5909 = FACE_OUTER_BOUND ( 'NONE', #739, .T. ) ;
#5910 = ORIENTED_EDGE ( 'NONE', *, *, #11303, .T. ) ;
#5911 = LINE ( 'NONE', #18464, #5139 ) ;
#5912 = PLANE ( 'NONE',  #15635 ) ;
#5913 = LINE ( 'NONE', #18468, #16653 ) ;
#5914 = DIRECTION ( 'NONE',  ( 0.000000000000000000, 0.000000000000000000, -1.000000000000000000 ) ) ;
#5915 = ORIENTED_EDGE ( 'NONE', *, *, #19947, .T. ) ;
#5916 = EDGE_LOOP ( 'NONE', ( #1568, #6955, #15573, #7260 ) ) ;
#5917 = CARTESIAN_POINT ( 'NONE',  ( 2.181929469893403528, 140.4048636633015406, 500.8237260975780600 ) ) ;
#5918 = PLANE ( 'NONE',  #9325 ) ;
#5919 = CIRCLE ( 'NONE', #11181, 1.000000000000000888 ) ;
#5920 = DIRECTION ( 'NONE',  ( 0.000000000000000000, 0.000000000000000000, 1.000000000000000000 ) ) ;
#5921 = STYLED_ITEM ( 'NONE', ( #7099 ), #6762 ) ;
#5922 = EDGE_CURVE ( 'NONE', #10337, #12769, #10537, .T. ) ;
#5923 = MECHANICAL_DESIGN_GEOMETRIC_PRESENTATION_REPRESENTATION (  '', ( #14467 ), #16145 ) ;
#5924 = ORIENTED_EDGE ( 'NONE', *, *, #16719, .T. ) ;
#5925 = EDGE_LOOP ( 'NONE', ( #4821, #5726 ) ) ;
#5926 = ORIENTED_EDGE ( 'NONE', *, *, #3344, .F. ) ;
#5927 = ORIENTED_EDGE ( 'NONE', *, *, #443, .T. ) ;
#5928 = DIRECTION ( 'NONE',  ( 1.000000000000000000, 0.000000000000000000, 0.000000000000000000 ) ) ;
#5929 = ORIENTED_EDGE ( 'NONE', *, *, #19943, .F. ) ;
#5930 = LINE ( 'NONE', #7491, #6398 ) ;
#5931 = CIRCLE ( 'NONE', #15823, 2.999999999999995559 ) ;
#5932 = PRESENTATION_STYLE_ASSIGNMENT (( #4200 ) ) ;
#5933 = SURFACE_SIDE_STYLE ('',( #20023 ) ) ;
#5934 = CARTESIAN_POINT ( 'NONE',  ( -81.18192946989243808, 139.7703989349477354, 490.5655098180907885 ) ) ;
#5935 = SURFACE_STYLE_USAGE ( .BOTH. , #12326 ) ;
#5936 = EDGE_CURVE ( 'NONE', #6700, #5100, #18426, .T. ) ;
#5937 = DIRECTION ( 'NONE',  ( 1.000000000000000000, 0.000000000000000000, 0.000000000000000000 ) ) ;
#5938 = FACE_OUTER_BOUND ( 'NONE', #7701, .T. ) ;
#5939 = CARTESIAN_POINT ( 'NONE',  ( 25.99999999999999645, 0.000000000000000000, 40.00000000000002132 ) ) ;
#5940 = FACE_OUTER_BOUND ( 'NONE', #19537, .T. ) ;
#5941 = CARTESIAN_POINT ( 'NONE',  ( 1.399999999999999911, 15.25000000000000000, 0.000000000000000000 ) ) ;
#5942 = PLANE ( 'NONE',  #3395 ) ;
#5943 = DIRECTION ( 'NONE',  ( -0.000000000000000000, -1.000000000000000000, -0.000000000000000000 ) ) ;
#5944 =( NAMED_UNIT ( * ) PLANE_ANGLE_UNIT ( ) SI_UNIT ( $, .RADIAN. ) );
#5945 = PLANE ( 'NONE',  #2010 ) ;
#5946 = DIRECTION ( 'NONE',  ( 0.000000000000000000, 0.000000000000000000, 1.000000000000000000 ) ) ;
#5947 = ORIENTED_EDGE ( 'NONE', *, *, #1132, .T. ) ;
#5948 = VECTOR ( 'NONE', #16928, 1000.000000000000000 ) ;
#5949 = EDGE_CURVE ( 'NONE', #1964, #11036, #9207, .T. ) ;
#5950 = ORIENTED_EDGE ( 'NONE', *, *, #5505, .F. ) ;
#5951 = ORIENTED_EDGE ( 'NONE', *, *, #19058, .F. ) ;
#5952 = PRODUCT_DEFINITION_SHAPE ( 'NONE', 'NONE',  #20375 ) ;
#5953 = VECTOR ( 'NONE', #16113, 1000.000000000000000 ) ;
#5954 = ORIENTED_EDGE ( 'NONE', *, *, #10655, .F. ) ;
#5955 = CARTESIAN_POINT ( 'NONE',  ( -26.00000000000002132, 10.00000000000000000, -39.99999999999999289 ) ) ;
#5956 = ORIENTED_EDGE ( 'NONE', *, *, #17325, .T. ) ;
#5957 = DIRECTION ( 'NONE',  ( 1.000000000000000000, 0.000000000000000000, 0.000000000000000000 ) ) ;
#5958 = DIRECTION ( 'NONE',  ( -0.000000000000000000, -1.000000000000000000, -0.000000000000000000 ) ) ;
#5959 = ORIENTED_EDGE ( 'NONE', *, *, #8103, .T. ) ;
#5960 = EDGE_CURVE ( 'NONE', #18280, #4081, #16804, .T. ) ;
#5961 = STYLED_ITEM ( 'NONE', ( #10151 ), #12040 ) ;
#5962 = CARTESIAN_POINT ( 'NONE',  ( 31.99999999999998579, 10.00000000000000000, 22.99999999999999645 ) ) ;
#5963 = AXIS2_PLACEMENT_3D ( 'NONE', #16294, #11624, #382 ) ;
#5964 = CARTESIAN_POINT ( 'NONE',  ( 111.4893729001366012, 129.7247684487574588, 283.6050404526570219 ) ) ;
#5965 = AXIS2_PLACEMENT_3D ( 'NONE', #8966, #15266, #1305 ) ;
#5966 = DIRECTION ( 'NONE',  ( 0.000000000000000000, 1.000000000000000000, 0.000000000000000000 ) ) ;
#5967 = FACE_OUTER_BOUND ( 'NONE', #12240, .T. ) ;
#5968 = DIRECTION ( 'NONE',  ( -1.000000000000000000, 0.000000000000000000, 0.000000000000000000 ) ) ;
#5969 = ADVANCED_FACE ( 'NONE', ( #1224, #5817, #2395, #8700, #12098 ), #853, .F. ) ;
#5970 = CARTESIAN_POINT ( 'NONE',  ( -35.00000000000000000, 19.00000000000000000, 20.99999999999999289 ) ) ;
#5971 =( NAMED_UNIT ( * ) SI_UNIT ( $, .STERADIAN. ) SOLID_ANGLE_UNIT ( ) );
#5972 = FILL_AREA_STYLE ('',( #9258 ) ) ;
#5973 = EDGE_CURVE ( 'NONE', #11681, #3507, #20, .T. ) ;
#5974 = ORIENTED_EDGE ( 'NONE', *, *, #10255, .T. ) ;
#5975 = MECHANICAL_DESIGN_GEOMETRIC_PRESENTATION_REPRESENTATION (  '', ( #12220 ), #4999 ) ;
#5976 = ORIENTED_EDGE ( 'NONE', *, *, #5403, .T. ) ;
#5977 = EDGE_CURVE ( 'NONE', #6311, #9122, #15824, .T. ) ;
#5978 = FACE_OUTER_BOUND ( 'NONE', #20185, .T. ) ;
#5979 = PRESENTATION_LAYER_ASSIGNMENT (  '', '', ( #5656 ) ) ;
#5980 = ORIENTED_EDGE ( 'NONE', *, *, #7129, .T. ) ;
#5981 = VERTEX_POINT ( 'NONE', #7855 ) ;
#5982 = PRESENTATION_STYLE_ASSIGNMENT (( #5887 ) ) ;
#5983 = EDGE_CURVE ( 'NONE', #7678, #6221, #15610, .T. ) ;
#5984 = CYLINDRICAL_SURFACE ( 'NONE', #1080, 10.00000000000000888 ) ;
#5985 = UNCERTAINTY_MEASURE_WITH_UNIT (LENGTH_MEASURE( 1.000000000000000082E-05 ), #8719, 'distance_accuracy_value', 'NONE');
#5986 = CARTESIAN_POINT ( 'NONE',  ( -211.5106270998635409, 113.1299228374912502, 220.6387154965113382 ) ) ;
#5987 = PLANE ( 'NONE',  #9178 ) ;
#5988 = EDGE_CURVE ( 'NONE', #10280, #19312, #3949, .T. ) ;
#5989 = SURFACE_STYLE_USAGE ( .BOTH. , #10524 ) ;
#5990 = FACE_OUTER_BOUND ( 'NONE', #19014, .T. ) ;
#5991 = CARTESIAN_POINT ( 'NONE',  ( 458.8334540492693350, 167.8734308960555950, 0.000000000000000000 ) ) ;
#5992 = EDGE_CURVE ( 'NONE', #15525, #5440, #11531, .T. ) ;
#5993 = VECTOR ( 'NONE', #12830, 1000.000000000000000 ) ;
#5994 = FACE_OUTER_BOUND ( 'NONE', #16237, .T. ) ;
#5995 = DIRECTION ( 'NONE',  ( 0.000000000000000000, 1.000000000000000000, 0.000000000000000000 ) ) ;
#5996 = CARTESIAN_POINT ( 'NONE',  ( -0.008242336927396939905, 139.6212446359134276, 500.5185750710210186 ) ) ;
#5997 = MECHANICAL_DESIGN_GEOMETRIC_PRESENTATION_REPRESENTATION (  '', ( #19147 ), #8622 ) ;
#5998 = EDGE_LOOP ( 'NONE', ( #19253, #7844, #8778, #14516 ) ) ;
#5999 = SURFACE_STYLE_USAGE ( .BOTH. , #11885 ) ;
#6000 = DIRECTION ( 'NONE',  ( 0.000000000000000000, 0.000000000000000000, 1.000000000000000000 ) ) ;
#6001 = EDGE_CURVE ( 'NONE', #11075, #15757, #18086, .T. ) ;
#6002 = AXIS2_PLACEMENT_3D ( 'NONE', #6587, #4723, #17602 ) ;
#6003 = ORIENTED_EDGE ( 'NONE', *, *, #10043, .F. ) ;
#6004 = VECTOR ( 'NONE', #6998, 1000.000000000000000 ) ;
#6005 = VECTOR ( 'NONE', #7694, 1000.000000000000000 ) ;
#6006 =( GEOMETRIC_REPRESENTATION_CONTEXT ( 3 ) GLOBAL_UNCERTAINTY_ASSIGNED_CONTEXT ( ( #8149 ) ) GLOBAL_UNIT_ASSIGNED_CONTEXT ( ( #16682, #1161, #13763 ) ) REPRESENTATION_CONTEXT ( 'NONE', 'WORKASPACE' ) );
#6007 = VERTEX_POINT ( 'NONE', #7957 ) ;
#6008 = EDGE_CURVE ( 'NONE', #9425, #11214, #4563, .T. ) ;
#6009 = LINE ( 'NONE', #19904, #17592 ) ;
#6010 = EDGE_LOOP ( 'NONE', ( #13835, #14000, #18533, #19877 ) ) ;
#6011 = DIRECTION ( 'NONE',  ( 0.000000000000000000, 0.000000000000000000, 1.000000000000000000 ) ) ;
#6012 =( LENGTH_UNIT ( ) NAMED_UNIT ( * ) SI_UNIT ( .MILLI., .METRE. ) );
#6013 = PRODUCT_DEFINITION_FORMATION_WITH_SPECIFIED_SOURCE ( 'ANY', '', #10900, .NOT_KNOWN. ) ;
#6014 = DIRECTION ( 'NONE',  ( 0.000000000000000000, 0.000000000000000000, -1.000000000000000000 ) ) ;
#6015 = EDGE_CURVE ( 'NONE', #15858, #21, #3123, .T. ) ;
#6016 = TOROIDAL_SURFACE ( 'NONE', #8003, 14.76997474683060041, 0.5250000000000000222 ) ;
#6017 = CIRCLE ( 'NONE', #6346, 1.000000000000000888 ) ;
#6018 = EDGE_CURVE ( 'NONE', #15834, #6700, #13940, .T. ) ;
#6019 = DIRECTION ( 'NONE',  ( -0.000000000000000000, -1.000000000000000000, -0.000000000000000000 ) ) ;
#6020 = LINE ( 'NONE', #15510, #13482 ) ;
#6021 = LINE ( 'NONE', #12194, #13018 ) ;
#6022 = VERTEX_POINT ( 'NONE', #18573 ) ;
#6023 = CARTESIAN_POINT ( 'NONE',  ( 2.181929469893301832, 138.7545334744432637, 500.8237260975780600 ) ) ;
#6024 = ORIENTED_EDGE ( 'NONE', *, *, #4640, .F. ) ;
#6025 =( NAMED_UNIT ( * ) PLANE_ANGLE_UNIT ( ) SI_UNIT ( $, .RADIAN. ) );
#6026 = CIRCLE ( 'NONE', #8343, 4.999999999999997335 ) ;
#6027 = VECTOR ( 'NONE', #4298, 1000.000000000000000 ) ;
#6028 = DIRECTION ( 'NONE',  ( 1.000000000000000000, 0.000000000000000000, 0.000000000000000000 ) ) ;
#6029 = ORIENTED_EDGE ( 'NONE', *, *, #7653, .F. ) ;
#6030 = ORIENTED_EDGE ( 'NONE', *, *, #1664, .T. ) ;
#6031 = EDGE_LOOP ( 'NONE', ( #17160, #1612, #15447, #4564 ) ) ;
#6032 = CLOSED_SHELL ( 'NONE', ( #6119, #4871, #9006, #9402, #10432, #8769, #13309, #6252, #19524, #5366, #16939, #17317, #11129, #5842, #6490, #12706, #5461, #12050 ) ) ;
#6033 = AXIS2_PLACEMENT_3D ( 'NONE', #234, #814, #8767 ) ;
#6034 = ORIENTED_EDGE ( 'NONE', *, *, #16724, .T. ) ;
#6035 = CARTESIAN_POINT ( 'NONE',  ( 21.99999999999998224, 8.000000000000000000, -32.99999999999999289 ) ) ;
#6036 = EDGE_LOOP ( 'NONE', ( #1976, #10814, #4832, #9399, #19918, #6652, #11186, #11120, #18798, #19954, #13382, #5108, #4749, #9542, #6175, #3075 ) ) ;
#6037 = VECTOR ( 'NONE', #12327, 1000.000000000000000 ) ;
#6038 = CARTESIAN_POINT ( 'NONE',  ( -3.000000000000000000, 6.000000000000000000, 22.00000000000000000 ) ) ;
#6039 = COLOUR_RGB ( '', 0.40784314, 0.44705882, 0.49803922) ;
#6040 = EDGE_LOOP ( 'NONE', ( #13426, #13266, #17909, #15322 ) ) ;
#6041 = CARTESIAN_POINT ( 'NONE',  ( 2.181929469892549545, 139.7545334744432637, 491.0690926367356042 ) ) ;
#6042 = ADVANCED_FACE ( 'NONE', ( #1326 ), #6220, .F. ) ;
#6043 = CARTESIAN_POINT ( 'NONE',  ( 406.3334540492693350, 167.8734308960555950, 250.0000000000000000 ) ) ;
#6044 = DIRECTION ( 'NONE',  ( 1.000000000000000000, 5.889072920838430686E-16, -0.000000000000000000 ) ) ;
#6045 = CARTESIAN_POINT ( 'NONE',  ( -75.00000000000000000, 368.2663108437010919, -87.78239810828596035 ) ) ;
#6046 = DIRECTION ( 'NONE',  ( -1.000000000000000000, -0.000000000000000000, -0.000000000000000000 ) ) ;
#6047 =( NAMED_UNIT ( * ) PLANE_ANGLE_UNIT ( ) SI_UNIT ( $, .RADIAN. ) );
#6048 = MECHANICAL_DESIGN_GEOMETRIC_PRESENTATION_REPRESENTATION (  '', ( #11652 ), #10324 ) ;
#6049 = AXIS2_PLACEMENT_3D ( 'NONE', #13256, #16265, #19507 ) ;
#6050 = LINE ( 'NONE', #7498, #13446 ) ;
#6051 = FILL_AREA_STYLE_COLOUR ( '', #1721 ) ;
#6052 = DIRECTION ( 'NONE',  ( -1.000000000000000000, -1.595148023886719315E-16, 0.000000000000000000 ) ) ;
#6053 = DIRECTION ( 'NONE',  ( 0.000000000000000000, -1.000000000000000000, 0.000000000000000000 ) ) ;
#6054 = DIRECTION ( 'NONE',  ( -6.123031769111888756E-17, 1.000000000000000000, 3.749151804555344967E-33 ) ) ;
#6055 = PLANE ( 'NONE',  #19707 ) ;
#6056 = DIRECTION ( 'NONE',  ( 0.000000000000000000, 1.000000000000000000, 0.000000000000000000 ) ) ;
#6057 = COLOUR_RGB ( '', 0.09019608, 0.27058824, 0.51372549) ;
#6058 = VERTEX_POINT ( 'NONE', #14444 ) ;
#6059 = STYLED_ITEM ( 'NONE', ( #4792 ), #19095 ) ;
#6060 = COLOUR_RGB ( '', 0.40784314, 0.44705882, 0.49803922) ;
#6061 = ORIENTED_EDGE ( 'NONE', *, *, #11236, .T. ) ;
#6062 = ORIENTED_EDGE ( 'NONE', *, *, #5234, .T. ) ;
#6063 =( GEOMETRIC_REPRESENTATION_CONTEXT ( 3 ) GLOBAL_UNCERTAINTY_ASSIGNED_CONTEXT ( ( #15086 ) ) GLOBAL_UNIT_ASSIGNED_CONTEXT ( ( #10448, #4268, #5706 ) ) REPRESENTATION_CONTEXT ( 'NONE', 'WORKASPACE' ) );
#6064 =( GEOMETRIC_REPRESENTATION_CONTEXT ( 3 ) GLOBAL_UNCERTAINTY_ASSIGNED_CONTEXT ( ( #16540 ) ) GLOBAL_UNIT_ASSIGNED_CONTEXT ( ( #19040, #11224, #4753 ) ) REPRESENTATION_CONTEXT ( 'NONE', 'WORKASPACE' ) );
#6065 = ORIENTED_EDGE ( 'NONE', *, *, #13533, .F. ) ;
#6066 = FACE_OUTER_BOUND ( 'NONE', #8934, .T. ) ;
#6067 = CARTESIAN_POINT ( 'NONE',  ( 40.00000000000001421, -3.000000000000000888, 0.000000000000000000 ) ) ;
#6068 = AXIS2_PLACEMENT_3D ( 'NONE', #8098, #20339, #6347 ) ;
#6069 = ORIENTED_EDGE ( 'NONE', *, *, #1946, .F. ) ;
#6070 = DIRECTION ( 'NONE',  ( 0.000000000000000000, 0.000000000000000000, -1.000000000000000000 ) ) ;
#6071 = EDGE_CURVE ( 'NONE', #7205, #13831, #2258, .T. ) ;
#6072 = SURFACE_STYLE_FILL_AREA ( #893 ) ;
#6073 = ORIENTED_EDGE ( 'NONE', *, *, #890, .T. ) ;
#6074 = AXIS2_PLACEMENT_3D ( 'NONE', #3568, #14382, #5219 ) ;
#6075 = AXIS2_PLACEMENT_3D ( 'NONE', #11575, #16138, #16434 ) ;
#6076 = DIRECTION ( 'NONE',  ( 5.551115123125777022E-14, 0.000000000000000000, -1.000000000000000000 ) ) ;
#6077 = COLOUR_RGB ( '', 0.31764706, 0.68627451, 0.89019608) ;
#6078 = CARTESIAN_POINT ( 'NONE',  ( 98.48937290013660117, 167.9162550801369491, -97.94896630388704750 ) ) ;
#6079 = CARTESIAN_POINT ( 'NONE',  ( -0.3928280596732490748, 62.98074339969887347, 9.493865254640493134 ) ) ;
#6080 = PRESENTATION_STYLE_ASSIGNMENT (( #13891 ) ) ;
#6081 = LINE ( 'NONE', #12366, #8349 ) ;
#6082 = CYLINDRICAL_SURFACE ( 'NONE', #19736, 4.999999999999997335 ) ;
#6083 = DIRECTION ( 'NONE',  ( 0.000000000000000000, 0.000000000000000000, -1.000000000000000000 ) ) ;
#6084 = TOROIDAL_SURFACE ( 'NONE', #12321, 8.000000000000000000, 1.000000000000000000 ) ;
#6085 = STYLED_ITEM ( 'NONE', ( #5932 ), #1009 ) ;
#6086 = PRESENTATION_STYLE_ASSIGNMENT (( #17011 ) ) ;
#6087 = PRESENTATION_STYLE_ASSIGNMENT (( #20176 ) ) ;
#6088 = STYLED_ITEM ( 'NONE', ( #9839 ), #10258 ) ;
#6089 = ADVANCED_FACE ( 'NONE', ( #14659 ), #226, .F. ) ;
#6090 =( GEOMETRIC_REPRESENTATION_CONTEXT ( 3 ) GLOBAL_UNCERTAINTY_ASSIGNED_CONTEXT ( ( #9914 ) ) GLOBAL_UNIT_ASSIGNED_CONTEXT ( ( #10354, #6966, #10451 ) ) REPRESENTATION_CONTEXT ( 'NONE', 'WORKASPACE' ) );
#6091 = COLOUR_RGB ( '', 0.31764706, 0.68627451, 0.89019608) ;
#6092 = ORIENTED_EDGE ( 'NONE', *, *, #9345, .T. ) ;
#6093 = ORIENTED_EDGE ( 'NONE', *, *, #8129, .F. ) ;
#6094 = EDGE_LOOP ( 'NONE', ( #11722, #19462, #4535, #15885 ) ) ;
#6095 = MECHANICAL_DESIGN_GEOMETRIC_PRESENTATION_REPRESENTATION (  '', ( #7403 ), #14634 ) ;
#6096 =( LENGTH_UNIT ( ) NAMED_UNIT ( * ) SI_UNIT ( .MILLI., .METRE. ) );
#6097 = ORIENTED_EDGE ( 'NONE', *, *, #5725, .T. ) ;
#6098 = ORIENTED_EDGE ( 'NONE', *, *, #7625, .T. ) ;
#6099 = VERTEX_POINT ( 'NONE', #2169 ) ;
#6100 = DIRECTION ( 'NONE',  ( -2.135044278125300850E-16, 1.000000000000000000, 0.000000000000000000 ) ) ;
#6101 = CARTESIAN_POINT ( 'NONE',  ( 1.181929469893326257, 216.7545334744432921, 500.8237260975781737 ) ) ;
#6102 = LINE ( 'NONE', #4441, #17473 ) ;
#6103 = MECHANICAL_DESIGN_GEOMETRIC_PRESENTATION_REPRESENTATION (  '', ( #8414 ), #17229 ) ;
#6105 = EDGE_CURVE ( 'NONE', #658, #15368, #5386, .T. ) ;
#6104 = CARTESIAN_POINT ( 'NONE',  ( -33.00000000000000000, 8.000000000000000000, -22.00000000000000355 ) ) ;
#6106 = CARTESIAN_POINT ( 'NONE',  ( 468.8334540492694487, 214.2156642432025251, 245.0000000000000000 ) ) ;
#6107 = MECHANICAL_DESIGN_GEOMETRIC_PRESENTATION_REPRESENTATION (  '', ( #13997 ), #5131 ) ;
#6108 = AXIS2_PLACEMENT_3D ( 'NONE', #8744, #12223, #3897 ) ;
#6109 = LINE ( 'NONE', #18660, #11675 ) ;
#6110 = CYLINDRICAL_SURFACE ( 'NONE', #3712, 4.999999999999997335 ) ;
#6111 = PLANE ( 'NONE',  #11609 ) ;
#6112 = AXIS2_PLACEMENT_3D ( 'NONE', #16500, #7126, #16611 ) ;
#6113 = ADVANCED_FACE ( 'NONE', ( #11359 ), #6632, .T. ) ;
#6114 = VERTEX_POINT ( 'NONE', #12920 ) ;
#6115 = CARTESIAN_POINT ( 'NONE',  ( 2.181929469893301832, 216.7545334744432921, 500.8237260975780600 ) ) ;
#6116 = FACE_OUTER_BOUND ( 'NONE', #4381, .T. ) ;
#6117 = EDGE_CURVE ( 'NONE', #1591, #8486, #11667, .T. ) ;
#6118 = COLOUR_RGB ( '', 0.66274510, 0.83137255, 0.94901961) ;
#6119 = ADVANCED_FACE ( 'NONE', ( #9817 ), #4582, .F. ) ;
#6120 = VERTEX_POINT ( 'NONE', #8376 ) ;
#6121 = ADVANCED_FACE ( 'NONE', ( #8474 ), #14752, .F. ) ;
#6122 = DIRECTION ( 'NONE',  ( 0.000000000000000000, 0.000000000000000000, -1.000000000000000000 ) ) ;
#6123 = ORIENTED_EDGE ( 'NONE', *, *, #5396, .F. ) ;
#6124 = SURFACE_SIDE_STYLE ('',( #18767 ) ) ;
#6125 = DIRECTION ( 'NONE',  ( 1.000000000000000000, -0.000000000000000000, 0.000000000000000000 ) ) ;
#6126 = ORIENTED_EDGE ( 'NONE', *, *, #3484, .F. ) ;
#6127 = SURFACE_SIDE_STYLE ('',( #4663 ) ) ;
#6128 = DIRECTION ( 'NONE',  ( 0.000000000000000000, 1.000000000000000000, 0.000000000000000000 ) ) ;
#6129 = AXIS2_PLACEMENT_3D ( 'NONE', #5064, #18955, #6611 ) ;
#6131 = EDGE_CURVE ( 'NONE', #10847, #5205, #12812, .T. ) ;
#6130 = DIRECTION ( 'NONE',  ( -5.551115123125782071E-14, 1.697225763491249802E-27, -1.000000000000000000 ) ) ;
#6132 = CIRCLE ( 'NONE', #14025, 2.500000000000002220 ) ;
#6133 = CARTESIAN_POINT ( 'NONE',  ( -0.8398228660021732628, 140.2112360712614532, 501.5757544859369546 ) ) ;
#6134 = CARTESIAN_POINT ( 'NONE',  ( 111.4893729001366012, 129.7247684487574304, 252.0000000000000000 ) ) ;
#6135 = CARTESIAN_POINT ( 'NONE',  ( 40.00000000000001421, 0.000000000000000000, -150.0000000000000000 ) ) ;
#6136 = LINE ( 'NONE', #9307, #17932 ) ;
#6137 = VERTEX_POINT ( 'NONE', #6844 ) ;
#6138 = CARTESIAN_POINT ( 'NONE',  ( 18.99999999999998224, 10.00000000000000000, -35.99999999999999289 ) ) ;
#6139 = PRESENTATION_STYLE_ASSIGNMENT (( #4481 ) ) ;
#6140 = DIRECTION ( 'NONE',  ( 0.000000000000000000, 0.000000000000000000, -1.000000000000000000 ) ) ;
#6141 = APPLICATION_PROTOCOL_DEFINITION ( 'draft international standard', 'automotive_design', 1998, #10922 ) ;
#6142 = EDGE_CURVE ( 'NONE', #7810, #11163, #19086, .T. ) ;
#6143 = ORIENTED_EDGE ( 'NONE', *, *, #11953, .F. ) ;
#6144 =( NAMED_UNIT ( * ) SI_UNIT ( $, .STERADIAN. ) SOLID_ANGLE_UNIT ( ) );
#6145 = ORIENTED_EDGE ( 'NONE', *, *, #9618, .T. ) ;
#6146 = EDGE_CURVE ( 'NONE', #12201, #3904, #3738, .T. ) ;
#6147 = VERTEX_POINT ( 'NONE', #10020 ) ;
#6148 = VECTOR ( 'NONE', #11755, 1000.000000000000000 ) ;
#6149 = EDGE_LOOP ( 'NONE', ( #9078, #139 ) ) ;
#6150 = AXIS2_PLACEMENT_3D ( 'NONE', #10487, #8938, #15239 ) ;
#6151 = CARTESIAN_POINT ( 'NONE',  ( 1.750000000000000000, 0.000000000000000000, 0.000000000000000000 ) ) ;
#6152 = VERTEX_POINT ( 'NONE', #3536 ) ;
#6153 = CARTESIAN_POINT ( 'NONE',  ( 0.5831304756500845787, 140.4822067609526925, 500.9113485223598445 ) ) ;
#6154 = VERTEX_POINT ( 'NONE', #14352 ) ;
#6155 = DIRECTION ( 'NONE',  ( -1.000000000000000000, -0.000000000000000000, -0.000000000000000000 ) ) ;
#6156 = CARTESIAN_POINT ( 'NONE',  ( -26.00000000000002842, 3.000000000000000000, -31.00000000000003197 ) ) ;
#6157 = FILL_AREA_STYLE_COLOUR ( '', #8545 ) ;
#6158 = PLANE ( 'NONE',  #18176 ) ;
#6159 = FACE_OUTER_BOUND ( 'NONE', #3417, .T. ) ;
#6160 = LINE ( 'NONE', #20029, #19055 ) ;
#6161 = EDGE_CURVE ( 'NONE', #7486, #1776, #8274, .T. ) ;
#6162 = DIRECTION ( 'NONE',  ( 0.000000000000000000, 1.000000000000000000, 0.000000000000000000 ) ) ;
#6163 = LINE ( 'NONE', #1803, #17507 ) ;
#6164 = LINE ( 'NONE', #18398, #2732 ) ;
#6165 = CIRCLE ( 'NONE', #11750, 2.500000000000002220 ) ;
#6166 = PLANE ( 'NONE',  #11361 ) ;
#6167 = CARTESIAN_POINT ( 'NONE',  ( 3.674999999999999822, 0.000000000000000000, 0.000000000000000000 ) ) ;
#6168 = FILL_AREA_STYLE ('',( #20040 ) ) ;
#6169 = EDGE_CURVE ( 'NONE', #625, #5490, #11828, .T. ) ;
#6170 = CARTESIAN_POINT ( 'NONE',  ( -1.000000000000012657, 139.2066006846527841, 488.2525619656395861 ) ) ;
#6171 = CARTESIAN_POINT ( 'NONE',  ( -26.00000000000000000, 19.00000000000000000, 40.00000000000001421 ) ) ;
#6172 = ADVANCED_FACE ( 'NONE', ( #3430 ), #14547, .F. ) ;
#6173 = ORIENTED_EDGE ( 'NONE', *, *, #16313, .F. ) ;
#6174 = EDGE_LOOP ( 'NONE', ( #7902, #11259, #16273, #9835 ) ) ;
#6175 = ORIENTED_EDGE ( 'NONE', *, *, #15467, .F. ) ;
#6176 = ORIENTED_EDGE ( 'NONE', *, *, #1627, .F. ) ;
#6177 = DIRECTION ( 'NONE',  ( 0.000000000000000000, -0.000000000000000000, 1.000000000000000000 ) ) ;
#6178 = CARTESIAN_POINT ( 'NONE',  ( -80.05917220250364608, 138.7922018492437530, 490.2440936989472675 ) ) ;
#6179 = EDGE_LOOP ( 'NONE', ( #18627, #13539, #19490, #10927 ) ) ;
#6180 = SHAPE_REPRESENTATION ( 'Part11^Assem2', ( #2741 ), #19153 ) ;
#6181 = CARTESIAN_POINT ( 'NONE',  ( 0.000000000000000000, 8.000000000000000000, -18.50000000000000000 ) ) ;
#6182 = VERTEX_POINT ( 'NONE', #16225 ) ;
#6183 = FACE_BOUND ( 'NONE', #2550, .T. ) ;
#6184 = FACE_OUTER_BOUND ( 'NONE', #2917, .T. ) ;
#6185 = ORIENTED_EDGE ( 'NONE', *, *, #1070, .T. ) ;
#6186 = DIRECTION ( 'NONE',  ( 1.000000000000000000, 0.000000000000000000, 0.000000000000000000 ) ) ;
#6187 = FILL_AREA_STYLE_COLOUR ( '', #1538 ) ;
#6188 = CARTESIAN_POINT ( 'NONE',  ( -26.00000000000002132, 0.000000000000000000, -39.99999999999999289 ) ) ;
#6189 = DIRECTION ( 'NONE',  ( 0.000000000000000000, 0.000000000000000000, -1.000000000000000000 ) ) ;
#6190 = FACE_BOUND ( 'NONE', #4241, .T. ) ;
#6191 = AXIS2_PLACEMENT_3D ( 'NONE', #11045, #17632, #6720 ) ;
#6192 = CARTESIAN_POINT ( 'NONE',  ( 0.000000000000000000, 50.00000000000000000, 0.000000000000000000 ) ) ;
#6193 = ADVANCED_FACE ( 'NONE', ( #2059 ), #19378, .T. ) ;
#6194 = VERTEX_POINT ( 'NONE', #8559 ) ;
#6195 = EDGE_LOOP ( 'NONE', ( #5836, #11775, #7732, #13663 ) ) ;
#6196 = ORIENTED_EDGE ( 'NONE', *, *, #11771, .T. ) ;
#6197 = CARTESIAN_POINT ( 'NONE',  ( 143.0892156028631348, 167.9162550801369491, 245.0000000000000000 ) ) ;
#6198 = ORIENTED_EDGE ( 'NONE', *, *, #18547, .T. ) ;
#6199 = ORIENTED_EDGE ( 'NONE', *, *, #3740, .F. ) ;
#6200 = ORIENTED_EDGE ( 'NONE', *, *, #6622, .T. ) ;
#6201 = CARTESIAN_POINT ( 'NONE',  ( 53.48937290013659407, 129.7247684487574588, 368.0000000000000000 ) ) ;
#6202 = PRESENTATION_STYLE_ASSIGNMENT (( #2984 ) ) ;
#6203 = LINE ( 'NONE', #9479, #684 ) ;
#6204 = DIRECTION ( 'NONE',  ( -1.000000000000000000, -0.000000000000000000, -0.000000000000000000 ) ) ;
#6205 = DIRECTION ( 'NONE',  ( -1.000000000000000000, 0.000000000000000000, -0.000000000000000000 ) ) ;
#6206 = CARTESIAN_POINT ( 'NONE',  ( 133.4893729001365443, 113.1299228374914634, 29.36128450348865471 ) ) ;
#6207 = LINE ( 'NONE', #7840, #16249 ) ;
#6208 = ADVANCED_FACE ( 'NONE', ( #7333 ), #721, .F. ) ;
#6209 =( LENGTH_UNIT ( ) NAMED_UNIT ( * ) SI_UNIT ( .MILLI., .METRE. ) );
#6210 = CARTESIAN_POINT ( 'NONE',  ( 31.00000000000006395, 68.00000000000000000, -22.99999999999999289 ) ) ;
#6211 = VERTEX_POINT ( 'NONE', #18035 ) ;
#6212 = DIRECTION ( 'NONE',  ( 0.7327934916262990317, 0.6804510993672779895, 0.000000000000000000 ) ) ;
#6213 = CIRCLE ( 'NONE', #6870, 4.999999999999997335 ) ;
#6214 = ADVANCED_FACE ( 'NONE', ( #8969 ), #13433, .F. ) ;
#6215 = VERTEX_POINT ( 'NONE', #10320 ) ;
#6216 = FACE_OUTER_BOUND ( 'NONE', #2891, .T. ) ;
#6217 = EDGE_CURVE ( 'NONE', #4888, #1517, #9223, .T. ) ;
#6218 = ORIENTED_EDGE ( 'NONE', *, *, #4607, .T. ) ;
#6219 = CARTESIAN_POINT ( 'NONE',  ( 55.48937290013659407, 208.2413221699789858, 346.7388812057777727 ) ) ;
#6220 = CYLINDRICAL_SURFACE ( 'NONE', #12513, 10.00000000000001066 ) ;
#6221 = VERTEX_POINT ( 'NONE', #11976 ) ;
#6222 = LINE ( 'NONE', #9300, #6393 ) ;
#6223 = CARTESIAN_POINT ( 'NONE',  ( -35.00000000000000000, 19.00000000000000000, 20.99999999999999289 ) ) ;
#6224 = AXIS2_PLACEMENT_3D ( 'NONE', #2071, #2383, #8393 ) ;
#6225 = CARTESIAN_POINT ( 'NONE',  ( 0.9068665838271406932, 139.7462607865923871, 500.8237261029128717 ) ) ;
#6226 = CARTESIAN_POINT ( 'NONE',  ( 20.99999999999996092, 3.000000000000000000, 37.50000000000001421 ) ) ;
#6227 = DIRECTION ( 'NONE',  ( 0.000000000000000000, 0.000000000000000000, 1.000000000000000000 ) ) ;
#6228 = PLANE ( 'NONE',  #15313 ) ;
#6229 = VERTEX_POINT ( 'NONE', #7448 ) ;
#6230 =( NAMED_UNIT ( * ) SI_UNIT ( $, .STERADIAN. ) SOLID_ANGLE_UNIT ( ) );
#6231 = EDGE_CURVE ( 'NONE', #19590, #14619, #974, .T. ) ;
#6232 = FACE_OUTER_BOUND ( 'NONE', #3446, .T. ) ;
#6233 = LINE ( 'NONE', #7780, #4415 ) ;
#6234 = EDGE_LOOP ( 'NONE', ( #18626, #13037 ) ) ;
#6235 = DIRECTION ( 'NONE',  ( -0.000000000000000000, 1.000000000000000000, -0.000000000000000000 ) ) ;
#6236 = EDGE_LOOP ( 'NONE', ( #3312, #10361, #4560, #7210 ) ) ;
#6237 = ORIENTED_EDGE ( 'NONE', *, *, #13819, .F. ) ;
#6238 = AXIS2_PLACEMENT_3D ( 'NONE', #5082, #17742, #6743 ) ;
#6239 = EDGE_CURVE ( 'NONE', #11766, #9619, #10429, .T. ) ;
#6240 = AXIS2_PLACEMENT_3D ( 'NONE', #13529, #17031, #5691 ) ;
#6241 = AXIS2_PLACEMENT_3D ( 'NONE', #15096, #9197, #19911 ) ;
#6242 = VERTEX_POINT ( 'NONE', #5889 ) ;
#6243 = EDGE_CURVE ( 'NONE', #20367, #1837, #10209, .T. ) ;
#6244 = ORIENTED_EDGE ( 'NONE', *, *, #15179, .T. ) ;
#6245 = DIRECTION ( 'NONE',  ( -0.000000000000000000, 1.000000000000000000, -0.000000000000000000 ) ) ;
#6246 = ORIENTED_EDGE ( 'NONE', *, *, #17446, .T. ) ;
#6247 = EDGE_CURVE ( 'NONE', #15316, #13471, #7939, .T. ) ;
#6248 = SURFACE_STYLE_FILL_AREA ( #7795 ) ;
#6249 = CARTESIAN_POINT ( 'NONE',  ( 31.00000000000000711, 0.000000000000000000, -30.99999999999999289 ) ) ;
#6250 = VECTOR ( 'NONE', #11625, 1000.000000000000000 ) ;
#6251 = FACE_BOUND ( 'NONE', #3974, .T. ) ;
#6252 = ADVANCED_FACE ( 'NONE', ( #4755 ), #5987, .F. ) ;
#6253 = CARTESIAN_POINT ( 'NONE',  ( 0.000000000000000000, 19.00100000000000122, 0.000000000000000000 ) ) ;
#6254 = AXIS2_PLACEMENT_3D ( 'NONE', #17721, #512, #605 ) ;
#6255 = CIRCLE ( 'NONE', #12171, 10.00000000000001066 ) ;
#6256 = DIRECTION ( 'NONE',  ( -0.000000000000000000, -1.000000000000000000, -0.000000000000000000 ) ) ;
#6257 = ORIENTED_EDGE ( 'NONE', *, *, #1249, .F. ) ;
#6258 = EDGE_CURVE ( 'NONE', #15622, #13610, #17746, .T. ) ;
#6259 = CARTESIAN_POINT ( 'NONE',  ( 26.00000000000001066, 68.00000000000000000, -31.00000000000002487 ) ) ;
#6260 = DIRECTION ( 'NONE',  ( 1.000000000000000000, -0.000000000000000000, 0.000000000000000000 ) ) ;
#6261 = LINE ( 'NONE', #6565, #9664 ) ;
#6262 =( NAMED_UNIT ( * ) SI_UNIT ( $, .STERADIAN. ) SOLID_ANGLE_UNIT ( ) );
#6263 = CARTESIAN_POINT ( 'NONE',  ( 98.48937290013662960, 1.571051285554951424E-14, 0.000000000000000000 ) ) ;
#6264 = FACE_BOUND ( 'NONE', #17003, .T. ) ;
#6265 = CARTESIAN_POINT ( 'NONE',  ( 31.81980515339464333, 0.000000000000000000, 31.81980515339463622 ) ) ;
#6266 = DIRECTION ( 'NONE',  ( 1.000000000000000000, 0.000000000000000000, 0.000000000000000000 ) ) ;
#6267 = ORIENTED_EDGE ( 'NONE', *, *, #4853, .T. ) ;
#6268 = AXIS2_PLACEMENT_3D ( 'NONE', #14085, #15855, #4706 ) ;
#6269 = VECTOR ( 'NONE', #5239, 1000.000000000000000 ) ;
#6270 = ORIENTED_EDGE ( 'NONE', *, *, #6239, .F. ) ;
#6271 = AXIS2_PLACEMENT_3D ( 'NONE', #16029, #1955, #17840 ) ;
#6272 = ORIENTED_EDGE ( 'NONE', *, *, #16378, .F. ) ;
#6273 = CARTESIAN_POINT ( 'NONE',  ( -80.29785759403569045, 140.6759013589731353, 501.1085235032808214 ) ) ;
#6274 = ORIENTED_EDGE ( 'NONE', *, *, #15171, .T. ) ;
#6275 = CARTESIAN_POINT ( 'NONE',  ( -38.50085094405407204, 193.0431417881923153, 510.3921618609452935 ) ) ;
#6276 = CARTESIAN_POINT ( 'NONE',  ( -211.5106270998635409, 113.1299228374912502, 29.36128450348865471 ) ) ;
#6277 = ORIENTED_EDGE ( 'NONE', *, *, #15595, .F. ) ;
#6278 = EDGE_CURVE ( 'NONE', #19193, #16250, #290, .T. ) ;
#6279 = CARTESIAN_POINT ( 'NONE',  ( 111.4893729001366012, 125.7247684487574588, 252.0000000000000000 ) ) ;
#6280 = CARTESIAN_POINT ( 'NONE',  ( -58.16843972078500258, 319.7545334744432353, 481.2863735482146126 ) ) ;
#6281 = DIRECTION ( 'NONE',  ( 7.715811803773179210E-14, 0.000000000000000000, 1.000000000000000000 ) ) ;
#6282 = ADVANCED_FACE ( 'NONE', ( #2785 ), #18544, .F. ) ;
#6283 = DIRECTION ( 'NONE',  ( 0.000000000000000000, 0.000000000000000000, 1.000000000000000000 ) ) ;
#6284 = EDGE_CURVE ( 'NONE', #10076, #4572, #12478, .T. ) ;
#6285 = FACE_OUTER_BOUND ( 'NONE', #3773, .T. ) ;
#6286 = LINE ( 'NONE', #18642, #10873 ) ;
#6287 = CIRCLE ( 'NONE', #17784, 10.00000000000000888 ) ;
#6288 = CARTESIAN_POINT ( 'NONE',  ( -23.00000000000003197, 3.000000000000000000, 34.00000000000000711 ) ) ;
#6289 = STYLED_ITEM ( 'NONE', ( #16234 ), #19856 ) ;
#6290 = CYLINDRICAL_SURFACE ( 'NONE', #18124, 0.9999999999999965583 ) ;
#6291 = CARTESIAN_POINT ( 'NONE',  ( 111.4893729001366012, 127.7247684487574588, 254.0000000000000000 ) ) ;
#6292 = VECTOR ( 'NONE', #18226, 1000.000000000000000 ) ;
#6293 = ORIENTED_EDGE ( 'NONE', *, *, #16438, .F. ) ;
#6294 = ORIENTED_EDGE ( 'NONE', *, *, #6771, .T. ) ;
#6295 = ORIENTED_EDGE ( 'NONE', *, *, #10417, .T. ) ;
#6296 = ORIENTED_EDGE ( 'NONE', *, *, #4236, .T. ) ;
#6297 = EDGE_LOOP ( 'NONE', ( #18126, #2622, #14627, #16997 ) ) ;
#6298 = DIRECTION ( 'NONE',  ( -9.815121534730717399E-17, 1.000000000000000000, 0.000000000000000000 ) ) ;
#6299 = VECTOR ( 'NONE', #2072, 1000.000000000000000 ) ;
#6300 = COLOUR_RGB ( '', 0.09019608, 0.27058824, 0.51372549) ;
#6301 = CARTESIAN_POINT ( 'NONE',  ( 5.044974746830580337, 0.000000000000000000, 0.000000000000000000 ) ) ;
#6302 = FACE_OUTER_BOUND ( 'NONE', #19846, .T. ) ;
#6303 = PRODUCT_DEFINITION_SHAPE ( 'NONE', 'NONE',  #17285 ) ;
#6304 = CARTESIAN_POINT ( 'NONE',  ( 78.48937290013661539, 80.91625508013694912, 0.000000000000000000 ) ) ;
#6305 = ADVANCED_FACE ( 'NONE', ( #18954 ), #20193, .F. ) ;
#6306 = DIRECTION ( 'NONE',  ( 0.000000000000000000, 1.000000000000000000, 0.000000000000000000 ) ) ;
#6307 = CARTESIAN_POINT ( 'NONE',  ( 486.8117674897343363, 214.2156642432025251, 245.0000000000000000 ) ) ;
#6308 = CARTESIAN_POINT ( 'NONE',  ( 133.4893729001365443, 103.1299228374914492, 170.4174721992565082 ) ) ;
#6309 = FACE_OUTER_BOUND ( 'NONE', #3510, .T. ) ;
#6310 = CARTESIAN_POINT ( 'NONE',  ( 0.3975717331714440639, 139.5287482107642631, 500.3163965736156911 ) ) ;
#6311 = VERTEX_POINT ( 'NONE', #3713 ) ;
#6312 = DIRECTION ( 'NONE',  ( -0.000000000000000000, -0.000000000000000000, -1.000000000000000000 ) ) ;
#6313 = FACE_OUTER_BOUND ( 'NONE', #4022, .T. ) ;
#6314 =( LENGTH_UNIT ( ) NAMED_UNIT ( * ) SI_UNIT ( .MILLI., .METRE. ) );
#6315 = ORIENTED_EDGE ( 'NONE', *, *, #4456, .T. ) ;
#6316 = APPLICATION_CONTEXT ( 'automotive_design' ) ;
#6317 = CYLINDRICAL_SURFACE ( 'NONE', #2983, 10.00000000000000888 ) ;
#6318 = ORIENTED_EDGE ( 'NONE', *, *, #14800, .F. ) ;
#6319 = DIRECTION ( 'NONE',  ( 0.000000000000000000, 1.000000000000000000, 0.000000000000000000 ) ) ;
#6320 = VECTOR ( 'NONE', #2108, 1000.000000000000000 ) ;
#6321 = VERTEX_POINT ( 'NONE', #17502 ) ;
#6322 =( NAMED_UNIT ( * ) SI_UNIT ( $, .STERADIAN. ) SOLID_ANGLE_UNIT ( ) );
#6323 = CARTESIAN_POINT ( 'NONE',  ( -19.00000000000001776, 10.00000000000000000, 40.00000000000000711 ) ) ;
#6324 = CARTESIAN_POINT ( 'NONE',  ( -31.00000000000001776, 0.000000000000000000, 31.00000000000000000 ) ) ;
#6325 = FACE_OUTER_BOUND ( 'NONE', #740, .T. ) ;
#6326 = DIRECTION ( 'NONE',  ( -0.000000000000000000, 1.000000000000000000, 0.000000000000000000 ) ) ;
#6327 = DIRECTION ( 'NONE',  ( 0.000000000000000000, 0.000000000000000000, -1.000000000000000000 ) ) ;
#6328 =( NAMED_UNIT ( * ) PLANE_ANGLE_UNIT ( ) SI_UNIT ( $, .RADIAN. ) );
#6329 = ORIENTED_EDGE ( 'NONE', *, *, #18466, .F. ) ;
#6330 =( LENGTH_UNIT ( ) NAMED_UNIT ( * ) SI_UNIT ( .MILLI., .METRE. ) );
#6331 = DIRECTION ( 'NONE',  ( 0.000000000000000000, 0.000000000000000000, 1.000000000000000000 ) ) ;
#6332 = SURFACE_SIDE_STYLE ('',( #33 ) ) ;
#6333 = SHAPE_DEFINITION_REPRESENTATION ( #8123, #18121 ) ;
#6334 = ORIENTED_EDGE ( 'NONE', *, *, #7017, .F. ) ;
#6335 = ORIENTED_EDGE ( 'NONE', *, *, #5973, .F. ) ;
#6336 = CARTESIAN_POINT ( 'NONE',  ( 98.48937290013662960, 123.1299228374914350, 170.4174721992565082 ) ) ;
#6337 = ORIENTED_EDGE ( 'NONE', *, *, #14822, .T. ) ;
#6338 = VECTOR ( 'NONE', #80, 1000.000000000000000 ) ;
#6339 = AXIS2_PLACEMENT_3D ( 'NONE', #14461, #1775, #11475 ) ;
#6340 = ORIENTED_EDGE ( 'NONE', *, *, #19817, .F. ) ;
#6341 = EDGE_LOOP ( 'NONE', ( #15203, #17145, #18172 ) ) ;
#6342 = EDGE_CURVE ( 'NONE', #16841, #19266, #206, .T. ) ;
#6343 = SURFACE_STYLE_FILL_AREA ( #16053 ) ;
#6344 = STYLED_ITEM ( 'NONE', ( #11204 ), #3060 ) ;
#6345 = ORIENTED_EDGE ( 'NONE', *, *, #561, .T. ) ;
#6346 = AXIS2_PLACEMENT_3D ( 'NONE', #12174, #16737, #7455 ) ;
#6347 = DIRECTION ( 'NONE',  ( 0.000000000000000000, 0.000000000000000000, 1.000000000000000000 ) ) ;
#6348 = ADVANCED_FACE ( 'NONE', ( #14524 ), #19453, .T. ) ;
#6349 = CYLINDRICAL_SURFACE ( 'NONE', #13532, 3.300000000000025135 ) ;
#6350 = ORIENTED_EDGE ( 'NONE', *, *, #1586, .T. ) ;
#6351 = DIRECTION ( 'NONE',  ( 0.000000000000000000, 1.000000000000000000, 0.000000000000000000 ) ) ;
#6352 = DIRECTION ( 'NONE',  ( 0.000000000000000000, -0.000000000000000000, -1.000000000000000000 ) ) ;
#6353 = AXIS2_PLACEMENT_3D ( 'NONE', #11191, #12442, #2847 ) ;
#6354 = CARTESIAN_POINT ( 'NONE',  ( 5.569974746830579804, 0.000000000000000000, 0.000000000000000000 ) ) ;
#6355 = FACE_OUTER_BOUND ( 'NONE', #16752, .T. ) ;
#6356 = EDGE_CURVE ( 'NONE', #13581, #9734, #9687, .T. ) ;
#6357 =( LENGTH_UNIT ( ) NAMED_UNIT ( * ) SI_UNIT ( .MILLI., .METRE. ) );
#6358 = VERTEX_POINT ( 'NONE', #5263 ) ;
#6359 =( LENGTH_UNIT ( ) NAMED_UNIT ( * ) SI_UNIT ( .MILLI., .METRE. ) );
#6360 = DIRECTION ( 'NONE',  ( 1.000000000000000000, 0.000000000000000000, -0.000000000000000000 ) ) ;
#6361 = LINE ( 'NONE', #12856, #8669 ) ;
#6362 = LINE ( 'NONE', #17165, #10378 ) ;
#6363 = CARTESIAN_POINT ( 'NONE',  ( 0.000000000000000000, 138.7723821175108014, 490.5025619657601510 ) ) ;
#6364 = VECTOR ( 'NONE', #1309, 1000.000000000000000 ) ;
#6365 = ADVANCED_FACE ( 'NONE', ( #395 ), #6825, .F. ) ;
#6366 = SURFACE_STYLE_USAGE ( .BOTH. , #1491 ) ;
#6367 = ORIENTED_EDGE ( 'NONE', *, *, #6448, .T. ) ;
#6368 = ADVANCED_FACE ( 'NONE', ( #16013 ), #9573, .F. ) ;
#6369 = CIRCLE ( 'NONE', #11626, 10.00000000000000888 ) ;
#6370 = EDGE_CURVE ( 'NONE', #10187, #3066, #5254, .T. ) ;
#6371 = ORIENTED_EDGE ( 'NONE', *, *, #7836, .F. ) ;
#6372 = PLANE ( 'NONE',  #17830 ) ;
#6373 = EDGE_CURVE ( 'NONE', #11362, #16195, #14737, .T. ) ;
#6374 = CARTESIAN_POINT ( 'NONE',  ( -79.59571519198017597, 139.7910723461943974, 500.8594560506689390 ) ) ;
#6375 = ORIENTED_EDGE ( 'NONE', *, *, #3714, .F. ) ;
#6376 = DIRECTION ( 'NONE',  ( 0.000000000000000000, 0.000000000000000000, 1.000000000000000000 ) ) ;
#6377 = DIRECTION ( 'NONE',  ( 1.000000000000000000, 0.000000000000000000, 0.000000000000000000 ) ) ;
#6378 = CLOSED_SHELL ( 'NONE', ( #18410, #14702, #5174, #18421, #19697, #11145, #5638, #11613, #8886, #3073, #12528, #9749 ) ) ;
#6379 = VERTEX_POINT ( 'NONE', #12795 ) ;
#6380 = CARTESIAN_POINT ( 'NONE',  ( 35.99999999999999289, 6.000000000000000000, 17.99999999999998934 ) ) ;
#6381 =( NAMED_UNIT ( * ) SI_UNIT ( $, .STERADIAN. ) SOLID_ANGLE_UNIT ( ) );
#6382 = DIRECTION ( 'NONE',  ( -1.000000000000000000, 0.000000000000000000, 0.000000000000000000 ) ) ;
#6383 = ADVANCED_FACE ( 'NONE', ( #5364 ), #6921, .T. ) ;
#6384 = CYLINDRICAL_SURFACE ( 'NONE', #4084, 10.00000000000000888 ) ;
#6385 = CARTESIAN_POINT ( 'NONE',  ( -21.00000000000002842, -20.00000000000000000, -34.99999999999999289 ) ) ;
#6386 = AXIS2_PLACEMENT_3D ( 'NONE', #15330, #8651, #18112 ) ;
#6387 = CIRCLE ( 'NONE', #8998, 3.283624802691453848 ) ;
#6388 = CARTESIAN_POINT ( 'NONE',  ( -26.00000000000002132, 10.00000000000000000, 40.00000000000000711 ) ) ;
#6389 = SURFACE_STYLE_USAGE ( .BOTH. , #4731 ) ;
#6390 = AXIS2_PLACEMENT_3D ( 'NONE', #3614, #17922, #3911 ) ;
#6391 = CARTESIAN_POINT ( 'NONE',  ( 498.8334540492693918, 191.8198460455371333, 225.0057801310552463 ) ) ;
#6392 = CARTESIAN_POINT ( 'NONE',  ( -37.00000000000000711, 10.00000000000000000, -18.00000000000000355 ) ) ;
#6393 = VECTOR ( 'NONE', #20112, 1000.000000000000000 ) ;
#6394 = LINE ( 'NONE', #9469, #4390 ) ;
#6395 = AXIS2_PLACEMENT_3D ( 'NONE', #11972, #5574, #15938 ) ;
#6396 = ADVANCED_FACE ( 'NONE', ( #15890 ), #1734, .F. ) ;
#6397 = VERTEX_POINT ( 'NONE', #11226 ) ;
#6398 = VECTOR ( 'NONE', #12034, 1000.000000000000000 ) ;
#6399 = ORIENTED_EDGE ( 'NONE', *, *, #2975, .F. ) ;
#6400 =( NAMED_UNIT ( * ) PLANE_ANGLE_UNIT ( ) SI_UNIT ( $, .RADIAN. ) );
#6401 = ORIENTED_EDGE ( 'NONE', *, *, #17417, .T. ) ;
#6402 = AXIS2_PLACEMENT_3D ( 'NONE', #20168, #10915, #1393 ) ;
#6403 = CIRCLE ( 'NONE', #10010, 8.000000000000000000 ) ;
#6404 = VERTEX_POINT ( 'NONE', #3408 ) ;
#6405 = DIRECTION ( 'NONE',  ( -0.000000000000000000, -1.000000000000000000, -0.000000000000000000 ) ) ;
#6406 = LINE ( 'NONE', #12694, #18564 ) ;
#6407 = AXIS2_PLACEMENT_3D ( 'NONE', #5296, #11886, #12756 ) ;
#6408 = CARTESIAN_POINT ( 'NONE',  ( 423.8334540492694487, 191.8198460455371333, 168.2339398819845826 ) ) ;
#6409 = CARTESIAN_POINT ( 'NONE',  ( -36.99999999999997868, -20.00000000000000000, -19.99999999999999289 ) ) ;
#6410 = CARTESIAN_POINT ( 'NONE',  ( -75.00000000000000000, 368.2663108437010919, -142.2176018917206761 ) ) ;
#6411 = AXIS2_PLACEMENT_3D ( 'NONE', #14998, #16947, #8806 ) ;
#6412 = CARTESIAN_POINT ( 'NONE',  ( -34.99999999999999289, 11.00000000000000000, -35.00000000000000711 ) ) ;
#6413 = CIRCLE ( 'NONE', #10336, 9.000000000000007105 ) ;
#6414 = DIRECTION ( 'NONE',  ( -1.000000000000000000, 0.000000000000000000, -0.000000000000000000 ) ) ;
#6415 = PRESENTATION_STYLE_ASSIGNMENT (( #14225 ) ) ;
#6416 = CARTESIAN_POINT ( 'NONE',  ( 143.0892156028631348, 80.91625508013694912, 245.0000000000000000 ) ) ;
#6417 = ORIENTED_EDGE ( 'NONE', *, *, #655, .T. ) ;
#6418 = ADVANCED_FACE ( 'NONE', ( #6609 ), #12900, .F. ) ;
#6419 = DIRECTION ( 'NONE',  ( -0.000000000000000000, -0.6449357872488783450, -0.7642367632649385012 ) ) ;
#6420 = CIRCLE ( 'NONE', #141, 2.999999999999999112 ) ;
#6421 = AXIS2_PLACEMENT_3D ( 'NONE', #14043, #3309, #17033 ) ;
#6422 = CARTESIAN_POINT ( 'NONE',  ( 4.025000000000000355, -17.52499999999999858, -2.146193515505736390E-15 ) ) ;
#6423 = VECTOR ( 'NONE', #15594, 1000.000000000000000 ) ;
#6424 = CIRCLE ( 'NONE', #9040, 10.00000000000000888 ) ;
#6425 = VECTOR ( 'NONE', #20288, 1000.000000000000000 ) ;
#6426 = ORIENTED_EDGE ( 'NONE', *, *, #17520, .F. ) ;
#6427 = STYLED_ITEM ( 'NONE', ( #11307 ), #10768 ) ;
#6428 = SURFACE_SIDE_STYLE ('',( #19066 ) ) ;
#6429 = ORIENTED_EDGE ( 'NONE', *, *, #2369, .T. ) ;
#6430 =( NAMED_UNIT ( * ) SI_UNIT ( $, .STERADIAN. ) SOLID_ANGLE_UNIT ( ) );
#6431 = ORIENTED_EDGE ( 'NONE', *, *, #3211, .T. ) ;
#6432 = DIRECTION ( 'NONE',  ( -0.000000000000000000, -0.000000000000000000, 1.000000000000000000 ) ) ;
#6433 = DIRECTION ( 'NONE',  ( 0.000000000000000000, 0.000000000000000000, -1.000000000000000000 ) ) ;
#6434 = AXIS2_PLACEMENT_3D ( 'NONE', #255, #11395, #9329 ) ;
#6435 = LINE ( 'NONE', #6223, #15315 ) ;
#6436 = CARTESIAN_POINT ( 'NONE',  ( 0.2985174824345476208, 140.6753058650092498, 501.1079383018479803 ) ) ;
#6437 = CARTESIAN_POINT ( 'NONE',  ( 78.48937290013660117, 113.1299228374914208, 170.4174721992565082 ) ) ;
#6438 = CARTESIAN_POINT ( 'NONE',  ( 2.999999999999996891, 60.00000000000000711, 6.000000000000000000 ) ) ;
#6439 = ORIENTED_EDGE ( 'NONE', *, *, #1240, .F. ) ;
#6440 = CARTESIAN_POINT ( 'NONE',  ( -31.00000000000006395, 3.000000000000000000, -25.99999999999999645 ) ) ;
#6441 = DIRECTION ( 'NONE',  ( 1.000000000000000000, -0.000000000000000000, -0.000000000000000000 ) ) ;
#6442 = FACE_OUTER_BOUND ( 'NONE', #8908, .T. ) ;
#6443 = AXIS2_PLACEMENT_3D ( 'NONE', #17058, #4492, #1053 ) ;
#6444 = ORIENTED_EDGE ( 'NONE', *, *, #17693, .F. ) ;
#6445 = PLANE ( 'NONE',  #4355 ) ;
#6446 = VERTEX_POINT ( 'NONE', #19857 ) ;
#6447 = VECTOR ( 'NONE', #7266, 1000.000000000000000 ) ;
#6448 = EDGE_CURVE ( 'NONE', #2599, #7013, #14828, .T. ) ;
#6449 = VERTEX_POINT ( 'NONE', #8648 ) ;
#6450 = CARTESIAN_POINT ( 'NONE',  ( 36.99999999999999289, 6.000000000000000000, 22.99999999999999645 ) ) ;
#6451 = ORIENTED_EDGE ( 'NONE', *, *, #18532, .F. ) ;
#6452 = CARTESIAN_POINT ( 'NONE',  ( -75.00000000000000000, 368.2663108437010919, -142.2176018917206761 ) ) ;
#6453 = DIRECTION ( 'NONE',  ( -6.123031769111888756E-17, -1.000000000000000000, 0.000000000000000000 ) ) ;
#6454 = AXIS2_PLACEMENT_3D ( 'NONE', #1205, #4438, #10616 ) ;
#6455 = DIRECTION ( 'NONE',  ( 0.000000000000000000, 0.000000000000000000, -1.000000000000000000 ) ) ;
#6456 = CARTESIAN_POINT ( 'NONE',  ( 498.8334540492693918, 167.8734308960555950, 250.0000000000000000 ) ) ;
#6457 = CARTESIAN_POINT ( 'NONE',  ( 0.000000000000000000, -5.000000000000000888, 0.000000000000000000 ) ) ;
#6458 = DIRECTION ( 'NONE',  ( -0.000000000000000000, -1.000000000000000000, -0.000000000000000000 ) ) ;
#6459 = DIRECTION ( 'NONE',  ( 0.000000000000000000, 0.000000000000000000, -1.000000000000000000 ) ) ;
#6460 = CARTESIAN_POINT ( 'NONE',  ( 1.181929469892510243, 139.7703989349544145, 490.5655098179848892 ) ) ;
#6461 = VERTEX_POINT ( 'NONE', #11642 ) ;
#6462 = CARTESIAN_POINT ( 'NONE',  ( 40.00000000000000711, 11.00000000000000000, 25.99999999999999645 ) ) ;
#6463 = EDGE_CURVE ( 'NONE', #72, #9120, #10191, .T. ) ;
#6464 = DIRECTION ( 'NONE',  ( -1.000000000000000000, 0.000000000000000000, -0.000000000000000000 ) ) ;
#6465 = CARTESIAN_POINT ( 'NONE',  ( -26.00000000000001776, 8.000000000000000000, 33.00000000000000711 ) ) ;
#6466 = DIRECTION ( 'NONE',  ( 0.000000000000000000, 1.000000000000000000, 0.000000000000000000 ) ) ;
#6467 = AXIS2_PLACEMENT_3D ( 'NONE', #1525, #9574, #9688 ) ;
#6468 =( NAMED_UNIT ( * ) SI_UNIT ( $, .STERADIAN. ) SOLID_ANGLE_UNIT ( ) );
#6469 = VERTEX_POINT ( 'NONE', #15044 ) ;
#6470 = PRESENTATION_LAYER_ASSIGNMENT (  '', '', ( #1171 ) ) ;
#6471 = EDGE_CURVE ( 'NONE', #10515, #11272, #19555, .T. ) ;
#6472 = ORIENTED_EDGE ( 'NONE', *, *, #4379, .F. ) ;
#6473 = CARTESIAN_POINT ( 'NONE',  ( 4.286263797015737285E-15, 0.000000000000000000, -35.00000000000000711 ) ) ;
#6474 = CARTESIAN_POINT ( 'NONE',  ( -81.00000000000085265, 139.7462607836631321, 500.8237260975782874 ) ) ;
#6475 = ORIENTED_EDGE ( 'NONE', *, *, #18968, .T. ) ;
#6476 = LINE ( 'NONE', #18815, #17266 ) ;
#6477 = EDGE_CURVE ( 'NONE', #8286, #18930, #10102, .T. ) ;
#6478 = ORIENTED_EDGE ( 'NONE', *, *, #16523, .T. ) ;
#6479 = DIRECTION ( 'NONE',  ( -1.000000000000000000, 0.000000000000000000, -0.000000000000000000 ) ) ;
#6480 = AXIS2_PLACEMENT_3D ( 'NONE', #17889, #957, #5839 ) ;
#6481 = FILL_AREA_STYLE ('',( #14195 ) ) ;
#6482 = PLANE ( 'NONE',  #18264 ) ;
#6483 = CARTESIAN_POINT ( 'NONE',  ( 1.163414457778310218E-15, 63.00000000000000000, 9.500000000000000000 ) ) ;
#6484 = DIRECTION ( 'NONE',  ( 1.000000000000000000, 0.000000000000000000, 0.000000000000000000 ) ) ;
#6485 = FILL_AREA_STYLE_COLOUR ( '', #7578 ) ;
#6486 = CARTESIAN_POINT ( 'NONE',  ( 10.00000000000000000, 381.0487089519826895, 2.719601036885452502E-12 ) ) ;
#6487 = DIRECTION ( 'NONE',  ( -0.000000000000000000, -1.000000000000000000, -0.000000000000000000 ) ) ;
#6488 = DIRECTION ( 'NONE',  ( -1.000000000000000000, 0.000000000000000000, 0.000000000000000000 ) ) ;
#6489 = CARTESIAN_POINT ( 'NONE',  ( 423.8334540492694487, 191.8198460455371333, 81.76606011801540319 ) ) ;
#6490 = ADVANCED_FACE ( 'NONE', ( #895 ), #18018, .F. ) ;
#6491 = ORIENTED_EDGE ( 'NONE', *, *, #10891, .T. ) ;
#6492 = ORIENTED_EDGE ( 'NONE', *, *, #20332, .T. ) ;
#6493 = UNCERTAINTY_MEASURE_WITH_UNIT (LENGTH_MEASURE( 1.000000000000000082E-05 ), #19627, 'distance_accuracy_value', 'NONE');
#6494 = EDGE_CURVE ( 'NONE', #3886, #8633, #8222, .T. ) ;
#6495 = DIRECTION ( 'NONE',  ( 1.000000000000000000, 0.000000000000000000, 0.000000000000000000 ) ) ;
#6496 = ORIENTED_EDGE ( 'NONE', *, *, #6117, .F. ) ;
#6497 = VERTEX_POINT ( 'NONE', #5775 ) ;
#6498 = VERTEX_POINT ( 'NONE', #11954 ) ;
#6499 = DIRECTION ( 'NONE',  ( 0.000000000000000000, 1.000000000000000000, 0.000000000000000000 ) ) ;
#6500 = SURFACE_STYLE_FILL_AREA ( #14331 ) ;
#6501 = CARTESIAN_POINT ( 'NONE',  ( 10.00000000000000000, 372.8685141053778693, -83.18019484660869978 ) ) ;
#6502 = CARTESIAN_POINT ( 'NONE',  ( 475.8334540492694487, 214.2156642432025251, 245.0000000000000000 ) ) ;
#6503 = CYLINDRICAL_SURFACE ( 'NONE', #13379, 4.999999999999997335 ) ;
#6504 = EDGE_CURVE ( 'NONE', #6007, #19270, #984, .T. ) ;
#6505 = ORIENTED_EDGE ( 'NONE', *, *, #9228, .F. ) ;
#6506 = CARTESIAN_POINT ( 'NONE',  ( 0.9999999999997842837, 139.4861549369088323, 500.2186618848270996 ) ) ;
#6507 = AXIS2_PLACEMENT_3D ( 'NONE', #3206, #8051, #6414 ) ;
#6508 = DIRECTION ( 'NONE',  ( 0.000000000000000000, 1.000000000000000000, 0.000000000000000000 ) ) ;
#6509 =( NAMED_UNIT ( * ) SI_UNIT ( $, .STERADIAN. ) SOLID_ANGLE_UNIT ( ) );
#6510 = ADVANCED_FACE ( 'NONE', ( #2350 ), #2463, .F. ) ;
#6511 = DIRECTION ( 'NONE',  ( 0.000000000000000000, 0.000000000000000000, -1.000000000000000000 ) ) ;
#6512 = SURFACE_STYLE_USAGE ( .BOTH. , #213 ) ;
#6513 = VERTEX_POINT ( 'NONE', #2658 ) ;
#6514 = FILL_AREA_STYLE_COLOUR ( '', #4106 ) ;
#6515 = FILL_AREA_STYLE ('',( #17116 ) ) ;
#6516 = AXIS2_PLACEMENT_3D ( 'NONE', #14247, #7963, #16036 ) ;
#6517 = ORIENTED_EDGE ( 'NONE', *, *, #17826, .F. ) ;
#6518 = FACE_BOUND ( 'NONE', #12788, .T. ) ;
#6519 = ORIENTED_EDGE ( 'NONE', *, *, #7005, .F. ) ;
#6520 = DIRECTION ( 'NONE',  ( 0.000000000000000000, 1.000000000000000000, 0.000000000000000000 ) ) ;
#6521 = VERTEX_POINT ( 'NONE', #5657 ) ;
#6522 = ADVANCED_FACE ( 'NONE', ( #8942 ), #18219, .T. ) ;
#6523 = DIRECTION ( 'NONE',  ( 1.000000000000000000, 0.000000000000000000, 0.000000000000000000 ) ) ;
#6524 = DIRECTION ( 'NONE',  ( 1.000000000000000000, 0.000000000000000000, 0.000000000000000000 ) ) ;
#6525 = ORIENTED_EDGE ( 'NONE', *, *, #5936, .T. ) ;
#6526 = DIRECTION ( 'NONE',  ( -0.000000000000000000, 1.000000000000000000, -0.000000000000000000 ) ) ;
#6527 = DIRECTION ( 'NONE',  ( -1.000000000000000000, -9.815121534730717399E-17, 0.000000000000000000 ) ) ;
#6528 = B_SPLINE_CURVE_WITH_KNOTS ( 'NONE', 3,
 ( #3959, #10348, #2605, #9109, #16543, #18273, #1137, #18157, #2398, #15397, #18465, #13542, #7171, #16659 ),
 .UNSPECIFIED., .F., .F.,
 ( 4, 2, 2, 2, 2, 2, 4 ),
 ( 0.000000000000000000, 0.0004665341218959795865, 0.0009330682437919591730, 0.001866136487584075772, 0.002332670609480022670, 0.002799204731375969351, 0.003732272975167592963 ),
 .UNSPECIFIED. ) ;
#6529 = DIRECTION ( 'NONE',  ( -0.000000000000000000, -1.000000000000000000, -0.000000000000000000 ) ) ;
#6530 = ADVANCED_FACE ( 'NONE', ( #1089, #13788, #17294, #15767, #20368 ), #12457, .F. ) ;
#6531 = CARTESIAN_POINT ( 'NONE',  ( 0.01793673982740404474, 141.2822582158146929, 501.5991098895786990 ) ) ;
#6532 = LINE ( 'NONE', #9506, #18339 ) ;
#6533 = FILL_AREA_STYLE_COLOUR ( '', #13983 ) ;
#6534 = CARTESIAN_POINT ( 'NONE',  ( 1.163414460601643398E-15, 38.00000000000000711, 9.500000000000000000 ) ) ;
#6535 = DIRECTION ( 'NONE',  ( -1.000000000000000000, 0.000000000000000000, 0.000000000000000000 ) ) ;
#6536 = AXIS2_PLACEMENT_3D ( 'NONE', #17572, #9532, #7996 ) ;
#6537 = ORIENTED_EDGE ( 'NONE', *, *, #15864, .F. ) ;
#6538 =( NAMED_UNIT ( * ) PLANE_ANGLE_UNIT ( ) SI_UNIT ( $, .RADIAN. ) );
#6539 = DIRECTION ( 'NONE',  ( 5.782411586589399054E-16, 0.000000000000000000, -1.000000000000000000 ) ) ;
#6540 = CARTESIAN_POINT ( 'NONE',  ( 22.99999999999999289, 68.00000000000000000, 37.00000000000002132 ) ) ;
#6541 = EDGE_CURVE ( 'NONE', #11558, #503, #14787, .T. ) ;
#6542 = CONTEXT_DEPENDENT_SHAPE_REPRESENTATION ( #12632, #17475 ) ;
#6543 = ORIENTED_EDGE ( 'NONE', *, *, #4890, .F. ) ;
#6544 = CARTESIAN_POINT ( 'NONE',  ( -37.00000000000000711, 10.00000000000000000, 23.00000000000000000 ) ) ;
#6545 = VERTEX_POINT ( 'NONE', #18636 ) ;
#6546 = ORIENTED_EDGE ( 'NONE', *, *, #2082, .F. ) ;
#6547 = ORIENTED_EDGE ( 'NONE', *, *, #5140, .T. ) ;
#6548 = VECTOR ( 'NONE', #4988, 1000.000000000000000 ) ;
#6549 = DIRECTION ( 'NONE',  ( 0.000000000000000000, 1.000000000000000000, 0.000000000000000000 ) ) ;
#6550 = ORIENTED_EDGE ( 'NONE', *, *, #3452, .F. ) ;
#6551 = DIRECTION ( 'NONE',  ( 1.000000000000000000, 0.000000000000000000, 0.000000000000000000 ) ) ;
#6552 = DIRECTION ( 'NONE',  ( 0.000000000000000000, 0.000000000000000000, -1.000000000000000000 ) ) ;
#6553 = CARTESIAN_POINT ( 'NONE',  ( 78.48937290013660117, 113.1299228374914208, 29.36128450348865471 ) ) ;
#6554 = DIRECTION ( 'NONE',  ( 0.000000000000000000, 0.000000000000000000, 1.000000000000000000 ) ) ;
#6555 = FACE_OUTER_BOUND ( 'NONE', #11003, .T. ) ;
#6556 = CARTESIAN_POINT ( 'NONE',  ( -79.99999999999995737, 140.1563709946295262, 488.5655098179835818 ) ) ;
#6557 = CARTESIAN_POINT ( 'NONE',  ( 153.4893729001366580, 80.91625508013694912, 0.000000000000000000 ) ) ;
#6558 = CARTESIAN_POINT ( 'NONE',  ( 178.4893729001365443, 145.9162550801369491, 250.0000000000000000 ) ) ;
#6559 = EDGE_CURVE ( 'NONE', #17453, #19090, #20028, .T. ) ;
#6560 = CARTESIAN_POINT ( 'NONE',  ( -2.694300560877699535, 39.66622868771214883, 9.110264267939502503 ) ) ;
#6561 = VERTEX_POINT ( 'NONE', #10909 ) ;
#6562 = PLANE ( 'NONE',  #9478 ) ;
#6563 =( LENGTH_UNIT ( ) NAMED_UNIT ( * ) SI_UNIT ( .MILLI., .METRE. ) );
#6564 = LINE ( 'NONE', #6786, #9292 ) ;
#6565 = CARTESIAN_POINT ( 'NONE',  ( 31.00000000000002842, 0.000000000000000000, 23.00000000000001066 ) ) ;
#6566 = DIRECTION ( 'NONE',  ( -0.000000000000000000, -1.000000000000000000, -0.000000000000000000 ) ) ;
#6567 = VECTOR ( 'NONE', #3615, 1000.000000000000000 ) ;
#6568 = AXIS2_PLACEMENT_3D ( 'NONE', #8142, #12992, #12883 ) ;
#6569 = ORIENTED_EDGE ( 'NONE', *, *, #3587, .T. ) ;
#6570 = DIRECTION ( 'NONE',  ( -1.000000000000000000, -0.000000000000000000, -0.000000000000000000 ) ) ;
#6571 = AXIS2_PLACEMENT_3D ( 'NONE', #8107, #17369, #19108 ) ;
#6572 = VERTEX_POINT ( 'NONE', #14005 ) ;
#6573 = VERTEX_POINT ( 'NONE', #5962 ) ;
#6574 = ORIENTED_EDGE ( 'NONE', *, *, #15524, .F. ) ;
#6575 = VERTEX_POINT ( 'NONE', #4314 ) ;
#6576 = DIRECTION ( 'NONE',  ( -1.135258727068399865E-15, -0.000000000000000000, 1.000000000000000000 ) ) ;
#6577 = CARTESIAN_POINT ( 'NONE',  ( -80.01784145024733164, 141.2836236309851188, 501.5999977085803039 ) ) ;
#6578 = COLOUR_RGB ( '', 0.31764706, 0.68627451, 0.89019608) ;
#6579 = EDGE_CURVE ( 'NONE', #8530, #10337, #16901, .T. ) ;
#6580 = VERTEX_POINT ( 'NONE', #10594 ) ;
#6581 = MECHANICAL_DESIGN_GEOMETRIC_PRESENTATION_REPRESENTATION (  '', ( #4922 ), #9528 ) ;
#6582 = FACE_OUTER_BOUND ( 'NONE', #669, .T. ) ;
#6583 = VECTOR ( 'NONE', #18713, 1000.000000000000000 ) ;
#6584 = COLOUR_RGB ( '', 0.66274510, 0.83137255, 0.94901961) ;
#6585 = ORIENTED_EDGE ( 'NONE', *, *, #11501, .T. ) ;
#6586 = CARTESIAN_POINT ( 'NONE',  ( 463.8334540492693350, 214.2156642432025251, -87.31255586191144857 ) ) ;
#6587 = CARTESIAN_POINT ( 'NONE',  ( 98.48937290013662960, 113.1299228374914350, 79.58252780074349175 ) ) ;
#6588 = LINE ( 'NONE', #10081, #19513 ) ;
#6589 = DIRECTION ( 'NONE',  ( -0.000000000000000000, -1.000000000000000000, -0.000000000000000000 ) ) ;
#6590 = DIRECTION ( 'NONE',  ( 1.000000000000000000, 0.000000000000000000, -0.000000000000000000 ) ) ;
#6591 = DIRECTION ( 'NONE',  ( -0.000000000000000000, -1.000000000000000000, -0.000000000000000000 ) ) ;
#6592 = ADVANCED_FACE ( 'NONE', ( #10805, #4722, #6183, #2859, #12241 ), #15672, .T. ) ;
#6593 = LINE ( 'NONE', #5045, #7545 ) ;
#6594 = CARTESIAN_POINT ( 'NONE',  ( 10.00000000000000000, 381.0487089519837127, -150.0000000000032685 ) ) ;
#6595 = SURFACE_STYLE_FILL_AREA ( #1832 ) ;
#6596 = AXIS2_PLACEMENT_3D ( 'NONE', #6897, #8518, #18088 ) ;
#6597 = AXIS2_PLACEMENT_3D ( 'NONE', #9192, #20109, #17338 ) ;
#6598 = PRODUCT_RELATED_PRODUCT_CATEGORY ( 'part', '', ( #208 ) ) ;
#6599 = ORIENTED_EDGE ( 'NONE', *, *, #85, .F. ) ;
#6600 = VERTEX_POINT ( 'NONE', #8228 ) ;
#6601 =( NAMED_UNIT ( * ) PLANE_ANGLE_UNIT ( ) SI_UNIT ( $, .RADIAN. ) );
#6602 = EDGE_LOOP ( 'NONE', ( #7286, #17443, #3549, #18096 ) ) ;
#6603 = ORIENTED_EDGE ( 'NONE', *, *, #12551, .F. ) ;
#6604 = EDGE_CURVE ( 'NONE', #11104, #14093, #3381, .T. ) ;
#6605 = ORIENTED_EDGE ( 'NONE', *, *, #11908, .F. ) ;
#6606 = DIRECTION ( 'NONE',  ( -0.000000000000000000, 1.000000000000000000, -0.000000000000000000 ) ) ;
#6607 = DIRECTION ( 'NONE',  ( 0.000000000000000000, 0.000000000000000000, -1.000000000000000000 ) ) ;
#6608 =( LENGTH_UNIT ( ) NAMED_UNIT ( * ) SI_UNIT ( .MILLI., .METRE. ) );
#6609 = FACE_OUTER_BOUND ( 'NONE', #4585, .T. ) ;
#6610 = CIRCLE ( 'NONE', #15507, 10.00000000000000888 ) ;
#6611 = DIRECTION ( 'NONE',  ( 0.000000000000000000, 1.000000000000000000, 0.000000000000000000 ) ) ;
#6612 = VECTOR ( 'NONE', #12064, 1000.000000000000000 ) ;
#6613 = AXIS2_PLACEMENT_3D ( 'NONE', #17345, #3228, #9507 ) ;
#6614 = VECTOR ( 'NONE', #13034, 1000.000000000000000 ) ;
#6615 = DIRECTION ( 'NONE',  ( -0.000000000000000000, 1.000000000000000000, -0.000000000000000000 ) ) ;
#6616 = PLANE ( 'NONE',  #10687 ) ;
#6617 = EDGE_CURVE ( 'NONE', #3904, #20015, #15866, .T. ) ;
#6618 = CARTESIAN_POINT ( 'NONE',  ( 31.00000000000003553, 0.000000000000000000, -23.00000000000000000 ) ) ;
#6619 = CARTESIAN_POINT ( 'NONE',  ( 40.00000000000001421, 0.000000000000000000, -150.0000000000000000 ) ) ;
#6620 = ADVANCED_FACE ( 'NONE', ( #19018 ), #14606, .T. ) ;
#6621 = LINE ( 'NONE', #17731, #11011 ) ;
#6622 = EDGE_CURVE ( 'NONE', #19448, #11484, #2628, .T. ) ;
#6623 = AXIS2_PLACEMENT_3D ( 'NONE', #15817, #4791, #12508 ) ;
#6624 = EDGE_CURVE ( 'NONE', #16461, #9346, #9658, .T. ) ;
#6625 = EDGE_LOOP ( 'NONE', ( #8796, #1613, #13962, #3505 ) ) ;
#6626 = FILL_AREA_STYLE ('',( #11352 ) ) ;
#6627 = ORIENTED_EDGE ( 'NONE', *, *, #6284, .T. ) ;
#6628 = EDGE_CURVE ( 'NONE', #4484, #693, #10196, .T. ) ;
#6629 = LINE ( 'NONE', #11355, #3662 ) ;
#6630 = ORIENTED_EDGE ( 'NONE', *, *, #7619, .F. ) ;
#6631 = CYLINDRICAL_SURFACE ( 'NONE', #16938, 36.50000000000000000 ) ;
#6632 = PLANE ( 'NONE',  #6271 ) ;
#6633 = ORIENTED_EDGE ( 'NONE', *, *, #11655, .F. ) ;
#6634 = DIRECTION ( 'NONE',  ( 0.000000000000000000, -1.000000000000000000, 0.000000000000000000 ) ) ;
#6635 = CARTESIAN_POINT ( 'NONE',  ( 25.99999999999997513, 0.000000000000000000, 31.00000000000003553 ) ) ;
#6636 = CARTESIAN_POINT ( 'NONE',  ( -25.99999999999999645, 68.00000000000000000, -31.00000000000003197 ) ) ;
#6637 = VECTOR ( 'NONE', #19759, 1000.000000000000000 ) ;
#6638 = CIRCLE ( 'NONE', #13540, 12.00000000000000000 ) ;
#6639 = CARTESIAN_POINT ( 'NONE',  ( 31.00000000000000711, 68.00000000000000000, -30.99999999999999289 ) ) ;
#6640 = CARTESIAN_POINT ( 'NONE',  ( 31.81980515339464333, 8.000000000000000000, 31.81980515339463622 ) ) ;
#6641 = CARTESIAN_POINT ( 'NONE',  ( 31.00000000000000000, 19.00000000000000000, -31.00000000000000355 ) ) ;
#6642 = CARTESIAN_POINT ( 'NONE',  ( 1.181929469892510243, 139.7703989349544145, 490.5655098179848892 ) ) ;
#6643 = EDGE_CURVE ( 'NONE', #7832, #9760, #10861, .T. ) ;
#6644 = VERTEX_POINT ( 'NONE', #14403 ) ;
#6645 = LINE ( 'NONE', #10131, #7214 ) ;
#6646 = CARTESIAN_POINT ( 'NONE',  ( 21.99999999999998224, 8.000000000000000000, -32.99999999999999289 ) ) ;
#6647 = ITEM_DEFINED_TRANSFORMATION ( 'NONE', 'NONE', #15226,  #2741 ) ;
#6648 = PRODUCT_DEFINITION_SHAPE ( 'NONE', 'NONE',  #20385 ) ;
#6649 = VERTEX_POINT ( 'NONE', #6688 ) ;
#6650 = CARTESIAN_POINT ( 'NONE',  ( 40.00000000000000711, 11.00000000000000000, -26.00000000000000355 ) ) ;
#6651 = EDGE_LOOP ( 'NONE', ( #8290, #10897 ) ) ;
#6652 = ORIENTED_EDGE ( 'NONE', *, *, #6847, .F. ) ;
#6653 = ORIENTED_EDGE ( 'NONE', *, *, #859, .T. ) ;
#6654 = EDGE_CURVE ( 'NONE', #2115, #1665, #14500, .T. ) ;
#6655 = VERTEX_POINT ( 'NONE', #15987 ) ;
#6656 = DIRECTION ( 'NONE',  ( -0.000000000000000000, -0.000000000000000000, 1.000000000000000000 ) ) ;
#6657 = EDGE_CURVE ( 'NONE', #10076, #2362, #3494, .T. ) ;
#6658 =( NAMED_UNIT ( * ) PLANE_ANGLE_UNIT ( ) SI_UNIT ( $, .RADIAN. ) );
#6659 = MECHANICAL_DESIGN_GEOMETRIC_PRESENTATION_REPRESENTATION (  '', ( #8941 ), #11238 ) ;
#6660 = EDGE_LOOP ( 'NONE', ( #18371, #14421, #12114, #13758 ) ) ;
#6661 = CARTESIAN_POINT ( 'NONE',  ( -211.5106270998635409, 103.1299228374912360, 29.36128450348865471 ) ) ;
#6662 = ADVANCED_FACE ( 'NONE', ( #8020 ), #17388, .T. ) ;
#6663 = CARTESIAN_POINT ( 'NONE',  ( 1.224999999999999867, 0.000000000000000000, 0.000000000000000000 ) ) ;
#6664 = ORIENTED_EDGE ( 'NONE', *, *, #876, .F. ) ;
#6665 = FACE_OUTER_BOUND ( 'NONE', #20237, .T. ) ;
#6666 =( NAMED_UNIT ( * ) SI_UNIT ( $, .STERADIAN. ) SOLID_ANGLE_UNIT ( ) );
#6667 = FACE_OUTER_BOUND ( 'NONE', #9431, .T. ) ;
#6668 = DIRECTION ( 'NONE',  ( 1.000000000000000000, -0.000000000000000000, -0.000000000000000000 ) ) ;
#6669 = CYLINDRICAL_SURFACE ( 'NONE', #11657, 1.000000000000000888 ) ;
#6670 = ORIENTED_EDGE ( 'NONE', *, *, #17199, .T. ) ;
#6671 = CARTESIAN_POINT ( 'NONE',  ( -15.00000000000000000, 316.7545334744432353, 495.1946179577816451 ) ) ;
#6672 = DIRECTION ( 'NONE',  ( 1.156482317317870344E-15, 0.000000000000000000, -1.000000000000000000 ) ) ;
#6673 = CIRCLE ( 'NONE', #18148, 10.00000000000000888 ) ;
#6674 = CARTESIAN_POINT ( 'NONE',  ( 0.000000000000000000, -5.000000000000000888, -150.0000000000000000 ) ) ;
#6675 =( LENGTH_UNIT ( ) NAMED_UNIT ( * ) SI_UNIT ( .MILLI., .METRE. ) );
#6676 = CARTESIAN_POINT ( 'NONE',  ( 423.8334540492694487, 191.8198460455371333, 81.76606011801540319 ) ) ;
#6677 = ORIENTED_EDGE ( 'NONE', *, *, #7535, .F. ) ;
#6678 = AXIS2_PLACEMENT_3D ( 'NONE', #12126, #7590, #2845 ) ;
#6679 = AXIS2_PLACEMENT_3D ( 'NONE', #18089, #14607, #19527 ) ;
#6680 = VERTEX_POINT ( 'NONE', #12771 ) ;
#6681 = EDGE_CURVE ( 'NONE', #11219, #17540, #13095, .T. ) ;
#6682 = VERTEX_POINT ( 'NONE', #278 ) ;
#6683 = LINE ( 'NONE', #12974, #18308 ) ;
#6684 = VECTOR ( 'NONE', #11495, 1000.000000000000000 ) ;
#6685 = VERTEX_POINT ( 'NONE', #9774 ) ;
#6686 = STYLED_ITEM ( 'NONE', ( #13388 ), #8244 ) ;
#6687 = ORIENTED_EDGE ( 'NONE', *, *, #1560, .T. ) ;
#6688 = CARTESIAN_POINT ( 'NONE',  ( -33.99999999999997158, 0.000000000000000000, -25.99999999999999645 ) ) ;
#6689 = CARTESIAN_POINT ( 'NONE',  ( -36.00000000000000711, 8.000000000000000000, -22.00000000000000355 ) ) ;
#6690 = CARTESIAN_POINT ( 'NONE',  ( 30.99999999999999645, 0.000000000000000000, -25.99999999999999645 ) ) ;
#6691 = DIRECTION ( 'NONE',  ( -0.000000000000000000, -1.000000000000000000, -0.000000000000000000 ) ) ;
#6692 = AXIS2_PLACEMENT_3D ( 'NONE', #3104, #13727, #19988 ) ;
#6693 = CARTESIAN_POINT ( 'NONE',  ( -20.00000000000003197, 0.000000000000000000, 37.00000000000000711 ) ) ;
#6694 = DIRECTION ( 'NONE',  ( -1.000000000000000000, 0.000000000000000000, 0.000000000000000000 ) ) ;
#6695 =( NAMED_UNIT ( * ) PLANE_ANGLE_UNIT ( ) SI_UNIT ( $, .RADIAN. ) );
#6696 = CARTESIAN_POINT ( 'NONE',  ( -30.99999999999999645, 68.00000000000000000, -30.99999999999999289 ) ) ;
#6697 = DIRECTION ( 'NONE',  ( -1.000000000000000000, 0.000000000000000000, 1.156482317317875472E-15 ) ) ;
#6698 = CARTESIAN_POINT ( 'NONE',  ( -15.00000000000000000, 317.7545334744432353, 495.1946179577816451 ) ) ;
#6699 = CIRCLE ( 'NONE', #7349, 10.00000000000000888 ) ;
#6700 = VERTEX_POINT ( 'NONE', #373 ) ;
#6701 = VECTOR ( 'NONE', #4816, 1000.000000000000000 ) ;
#6702 = FILL_AREA_STYLE_COLOUR ( '', #6118 ) ;
#6703 = VERTEX_POINT ( 'NONE', #3277 ) ;
#6704 = ORIENTED_EDGE ( 'NONE', *, *, #12967, .T. ) ;
#6705 = ADVANCED_FACE ( 'NONE', ( #11203 ), #16085, .F. ) ;
#6706 = CIRCLE ( 'NONE', #16907, 14.59999999999999964 ) ;
#6707 = EDGE_LOOP ( 'NONE', ( #7346, #5788 ) ) ;
#6708 =( GEOMETRIC_REPRESENTATION_CONTEXT ( 3 ) GLOBAL_UNCERTAINTY_ASSIGNED_CONTEXT ( ( #11943 ) ) GLOBAL_UNIT_ASSIGNED_CONTEXT ( ( #6996, #3693, #5157 ) ) REPRESENTATION_CONTEXT ( 'NONE', 'WORKASPACE' ) );
#6709 = ORIENTED_EDGE ( 'NONE', *, *, #6373, .F. ) ;
#6710 = LINE ( 'NONE', #18950, #12379 ) ;
#6711 = SURFACE_STYLE_FILL_AREA ( #16201 ) ;
#6712 = CARTESIAN_POINT ( 'NONE',  ( 10.00000000000000000, 376.0487089519837127, -155.0000000000033253 ) ) ;
#6713 = CIRCLE ( 'NONE', #18858, 10.00000000000000888 ) ;
#6714 = VECTOR ( 'NONE', #10887, 1000.000000000000000 ) ;
#6715 = DIRECTION ( 'NONE',  ( 0.000000000000000000, 1.000000000000000000, 0.000000000000000000 ) ) ;
#6716 = CARTESIAN_POINT ( 'NONE',  ( 35.00000000000003553, 3.000000000000000000, -23.50000000000000000 ) ) ;
#6717 = CIRCLE ( 'NONE', #20188, 34.00000000000000000 ) ;
#6718 = CARTESIAN_POINT ( 'NONE',  ( -26.00000000000002132, 0.000000000000000000, 40.00000000000000711 ) ) ;
#6719 = CARTESIAN_POINT ( 'NONE',  ( 2.600106608147765286, 61.50910620841189314, 9.137947797636652325 ) ) ;
#6720 = DIRECTION ( 'NONE',  ( 3.392348130799086764E-14, 0.000000000000000000, -1.000000000000000000 ) ) ;
#6721 =( REPRESENTATION_RELATIONSHIP ('NONE','NONE', #13279, #17354 ) REPRESENTATION_RELATIONSHIP_WITH_TRANSFORMATION ( #9605 )SHAPE_REPRESENTATION_RELATIONSHIP( ) );
#6722 =( LENGTH_UNIT ( ) NAMED_UNIT ( * ) SI_UNIT ( .MILLI., .METRE. ) );
#6723 = CARTESIAN_POINT ( 'NONE',  ( -78.99999999999995737, 141.3905724437643414, 503.0282008302663144 ) ) ;
#6724 = LINE ( 'NONE', #15896, #15252 ) ;
#6725 = AXIS2_PLACEMENT_3D ( 'NONE', #8102, #14379, #3767 ) ;
#6726 =( GEOMETRIC_REPRESENTATION_CONTEXT ( 3 ) GLOBAL_UNCERTAINTY_ASSIGNED_CONTEXT ( ( #15296 ) ) GLOBAL_UNIT_ASSIGNED_CONTEXT ( ( #15887, #18952, #9477 ) ) REPRESENTATION_CONTEXT ( 'NONE', 'WORKASPACE' ) );
#6727 = AXIS2_PLACEMENT_3D ( 'NONE', #5852, #19837, #12222 ) ;
#6728 = CARTESIAN_POINT ( 'NONE',  ( 78.48937290013660117, 113.1299228374914208, 79.58252780074349175 ) ) ;
#6729 = EDGE_CURVE ( 'NONE', #4741, #1482, #8332, .T. ) ;
#6730 = CARTESIAN_POINT ( 'NONE',  ( -15.00000000000000000, 317.7545334744432353, 495.1946179577816451 ) ) ;
#6731 = CIRCLE ( 'NONE', #15940, 3.300000000000000711 ) ;
#6732 = MECHANICAL_DESIGN_GEOMETRIC_PRESENTATION_REPRESENTATION (  '', ( #1415 ), #14287 ) ;
#6733 = MECHANICAL_DESIGN_GEOMETRIC_PRESENTATION_REPRESENTATION (  '', ( #9668 ), #9343 ) ;
#6734 = ORIENTED_EDGE ( 'NONE', *, *, #19425, .T. ) ;
#6735 = VECTOR ( 'NONE', #8797, 1000.000000000000000 ) ;
#6736 = DIRECTION ( 'NONE',  ( -0.000000000000000000, -1.000000000000000000, 0.000000000000000000 ) ) ;
#6737 = EDGE_LOOP ( 'NONE', ( #13402, #573, #16102, #9549 ) ) ;
#6738 = MECHANICAL_DESIGN_GEOMETRIC_PRESENTATION_REPRESENTATION (  '', ( #11651 ), #6063 ) ;
#6739 = EDGE_CURVE ( 'NONE', #14517, #11944, #11515, .T. ) ;
#6740 = CARTESIAN_POINT ( 'NONE',  ( -211.5106270998635409, 113.1299228374912502, 29.36128450348865471 ) ) ;
#6741 = ORIENTED_EDGE ( 'NONE', *, *, #294, .F. ) ;
#6742 = PLANE ( 'NONE',  #19248 ) ;
#6743 = DIRECTION ( 'NONE',  ( 0.000000000000000000, 1.000000000000000000, 0.000000000000000000 ) ) ;
#6744 = ORIENTED_EDGE ( 'NONE', *, *, #18242, .T. ) ;
#6745 = CIRCLE ( 'NONE', #5408, 2.999999999999999112 ) ;
#6746 = FACE_OUTER_BOUND ( 'NONE', #18883, .T. ) ;
#6747 = CARTESIAN_POINT ( 'NONE',  ( -1.000000000000000888, 216.7545334744432921, 477.3411705753777596 ) ) ;
#6748 = DIRECTION ( 'NONE',  ( 0.000000000000000000, 1.000000000000000000, 0.000000000000000000 ) ) ;
#6749 = ADVANCED_FACE ( 'NONE', ( #2126 ), #8439, .F. ) ;
#6750 = VECTOR ( 'NONE', #19226, 1000.000000000000000 ) ;
#6751 = VECTOR ( 'NONE', #5785, 1000.000000000000000 ) ;
#6752 =( GEOMETRIC_REPRESENTATION_CONTEXT ( 3 ) GLOBAL_UNCERTAINTY_ASSIGNED_CONTEXT ( ( #11557 ) ) GLOBAL_UNIT_ASSIGNED_CONTEXT ( ( #4182, #15188, #4269 ) ) REPRESENTATION_CONTEXT ( 'NONE', 'WORKASPACE' ) );
#6753 = CARTESIAN_POINT ( 'NONE',  ( 35.00000000000003553, 0.000000000000000000, -18.49999999999999645 ) ) ;
#6754 = CARTESIAN_POINT ( 'NONE',  ( 178.4893729001366012, 34.32473510485366575, 250.0000000000000000 ) ) ;
#6755 = LINE ( 'NONE', #16429, #5611 ) ;
#6756 = STYLED_ITEM ( 'NONE', ( #9489 ), #15873 ) ;
#6757 = SURFACE_STYLE_USAGE ( .BOTH. , #13046 ) ;
#6758 = VERTEX_POINT ( 'NONE', #5742 ) ;
#6759 = FILL_AREA_STYLE ('',( #9827 ) ) ;
#6760 = DIRECTION ( 'NONE',  ( 0.000000000000000000, 0.000000000000000000, -1.000000000000000000 ) ) ;
#6761 = DIRECTION ( 'NONE',  ( 1.000000000000000000, 0.000000000000000000, 0.000000000000000000 ) ) ;
#6762 = ADVANCED_FACE ( 'NONE', ( #8735 ), #5535, .T. ) ;
#6763 = VECTOR ( 'NONE', #13336, 1000.000000000000000 ) ;
#6764 = CARTESIAN_POINT ( 'NONE',  ( 31.00000000000000000, 8.000000000000000000, -31.00000000000000355 ) ) ;
#6765 = EDGE_CURVE ( 'NONE', #13737, #17589, #16473, .T. ) ;
#6766 = VECTOR ( 'NONE', #6319, 1000.000000000000000 ) ;
#6767 = ORIENTED_EDGE ( 'NONE', *, *, #8849, .T. ) ;
#6768 = ORIENTED_EDGE ( 'NONE', *, *, #11088, .T. ) ;
#6769 = DIRECTION ( 'NONE',  ( 0.000000000000000000, 0.000000000000000000, 1.000000000000000000 ) ) ;
#6770 = AXIS2_PLACEMENT_3D ( 'NONE', #20027, #7687, #4387 ) ;
#6771 = EDGE_CURVE ( 'NONE', #17991, #13550, #2633, .T. ) ;
#6772 = ORIENTED_EDGE ( 'NONE', *, *, #18698, .F. ) ;
#6773 = FACE_OUTER_BOUND ( 'NONE', #13878, .T. ) ;
#6774 = CARTESIAN_POINT ( 'NONE',  ( 3.000000000000000888, 40.80033764248782546, 9.013878188659974811 ) ) ;
#6775 = EDGE_LOOP ( 'NONE', ( #12739, #18964, #2753, #20264 ) ) ;
#6776 = SURFACE_SIDE_STYLE ('',( #13246 ) ) ;
#6777 = CARTESIAN_POINT ( 'NONE',  ( -40.00000000000000711, 0.000000000000000000, -26.00000000000000000 ) ) ;
#6778 = CIRCLE ( 'NONE', #4737, 8.000000000000007105 ) ;
#6779 = CARTESIAN_POINT ( 'NONE',  ( 6.649999999999999467, 0.000000000000000000, 0.000000000000000000 ) ) ;
#6780 = EDGE_CURVE ( 'NONE', #19519, #10459, #3984, .T. ) ;
#6781 = CYLINDRICAL_SURFACE ( 'NONE', #2919, 10.00000000000000888 ) ;
#6782 = DIRECTION ( 'NONE',  ( 0.000000000000000000, 0.000000000000000000, -1.000000000000000000 ) ) ;
#6783 = ORIENTED_EDGE ( 'NONE', *, *, #7142, .T. ) ;
#6784 = DIRECTION ( 'NONE',  ( 0.000000000000000000, 1.000000000000000000, 0.000000000000000000 ) ) ;
#6785 = SURFACE_STYLE_FILL_AREA ( #5132 ) ;
#6786 = CARTESIAN_POINT ( 'NONE',  ( -31.81980515339462912, 8.000000000000000000, -28.51980515339464972 ) ) ;
#6787 = EDGE_CURVE ( 'NONE', #9381, #12056, #11729, .T. ) ;
#6788 = CIRCLE ( 'NONE', #180, 3.883636366625808911 ) ;
#6789 = DIRECTION ( 'NONE',  ( -0.000000000000000000, -1.000000000000000000, 0.000000000000000000 ) ) ;
#6790 = LINE ( 'NONE', #1998, #12168 ) ;
#6791 = EDGE_LOOP ( 'NONE', ( #16556, #16142, #2018, #12518, #17552 ) ) ;
#6792 =( GEOMETRIC_REPRESENTATION_CONTEXT ( 3 ) GLOBAL_UNCERTAINTY_ASSIGNED_CONTEXT ( ( #3537 ) ) GLOBAL_UNIT_ASSIGNED_CONTEXT ( ( #6314, #12291, #6322 ) ) REPRESENTATION_CONTEXT ( 'NONE', 'WORKASPACE' ) );
#6793 = VERTEX_POINT ( 'NONE', #15115 ) ;
#6794 = VECTOR ( 'NONE', #18383, 1000.000000000000000 ) ;
#6795 = EDGE_LOOP ( 'NONE', ( #13222, #19272, #1148, #18741 ) ) ;
#6796 = SURFACE_SIDE_STYLE ('',( #2214 ) ) ;
#6797 = DIRECTION ( 'NONE',  ( 0.000000000000000000, -0.9497703099767278445, -0.3129478523439812032 ) ) ;
#6798 = ORIENTED_EDGE ( 'NONE', *, *, #4440, .T. ) ;
#6799 =( NAMED_UNIT ( * ) PLANE_ANGLE_UNIT ( ) SI_UNIT ( $, .RADIAN. ) );
#6800 = PRESENTATION_STYLE_ASSIGNMENT (( #14912 ) ) ;
#6801 = EDGE_CURVE ( 'NONE', #9471, #3904, #10166, .T. ) ;
#6802 = ORIENTED_EDGE ( 'NONE', *, *, #9833, .T. ) ;
#6803 = CARTESIAN_POINT ( 'NONE',  ( -75.00000000000000000, 313.8311070602663904, -142.2176018917206761 ) ) ;
#6804 = CARTESIAN_POINT ( 'NONE',  ( 40.00000000000001421, 3.000000000000000888, -150.0000000000000000 ) ) ;
#6805 = CARTESIAN_POINT ( 'NONE',  ( 0.02413213198956416089, 140.0034334293438292, 488.8196209980684444 ) ) ;
#6806 = FACE_OUTER_BOUND ( 'NONE', #427, .T. ) ;
#6807 = ADVANCED_FACE ( 'NONE', ( #11614 ), #873, .T. ) ;
#6808 = CARTESIAN_POINT ( 'NONE',  ( 53.48937290013658696, 103.1299228374913923, 29.36128450348865471 ) ) ;
#6809 = EDGE_CURVE ( 'NONE', #10453, #7117, #16160, .T. ) ;
#6810 = VECTOR ( 'NONE', #7630, 1000.000000000000000 ) ;
#6811 = CARTESIAN_POINT ( 'NONE',  ( 10.00000000000000000, 309.2289037985890445, -150.1198051533984597 ) ) ;
#6812 = DIRECTION ( 'NONE',  ( 1.000000000000000000, 5.889072920838430686E-16, -0.000000000000000000 ) ) ;
#6813 = DIRECTION ( 'NONE',  ( 1.156482317317875472E-15, 0.000000000000000000, 1.000000000000000000 ) ) ;
#6814 = LINE ( 'NONE', #6907, #16200 ) ;
#6815 = FILL_AREA_STYLE ('',( #16095 ) ) ;
#6816 = ORIENTED_EDGE ( 'NONE', *, *, #370, .F. ) ;
#6817 = ORIENTED_EDGE ( 'NONE', *, *, #85, .T. ) ;
#6818 = ORIENTED_EDGE ( 'NONE', *, *, #9513, .T. ) ;
#6819 = VECTOR ( 'NONE', #19454, 1000.000000000000000 ) ;
#6820 = ORIENTED_EDGE ( 'NONE', *, *, #4117, .F. ) ;
#6821 = ORIENTED_EDGE ( 'NONE', *, *, #6920, .T. ) ;
#6822 = LINE ( 'NONE', #19273, #2176 ) ;
#6823 = DIRECTION ( 'NONE',  ( 0.000000000000000000, 0.000000000000000000, -1.000000000000000000 ) ) ;
#6824 = CARTESIAN_POINT ( 'NONE',  ( 25.99999999999997868, 10.00000000000000000, 40.00000000000000711 ) ) ;
#6825 = CYLINDRICAL_SURFACE ( 'NONE', #18071, 3.000000000000002665 ) ;
#6826 = FILL_AREA_STYLE ('',( #15045 ) ) ;
#6827 = CARTESIAN_POINT ( 'NONE',  ( 35.00000000000003553, 0.000000000000000000, -20.99999999999999645 ) ) ;
#6828 = FACE_BOUND ( 'NONE', #2832, .T. ) ;
#6829 = FILL_AREA_STYLE ('',( #14432 ) ) ;
#6830 = CARTESIAN_POINT ( 'NONE',  ( -3.000000000000000000, -1.836909530733565148E-16, 12.50000000000000000 ) ) ;
#6831 = CARTESIAN_POINT ( 'NONE',  ( -79.99999999999995737, 146.8256012863087676, 480.6843163258853906 ) ) ;
#6832 = LINE ( 'NONE', #4960, #2388 ) ;
#6833 = EDGE_CURVE ( 'NONE', #10459, #7754, #2430, .T. ) ;
#6834 = DIRECTION ( 'NONE',  ( 0.000000000000000000, 0.000000000000000000, -1.000000000000000000 ) ) ;
#6835 = ORIENTED_EDGE ( 'NONE', *, *, #6018, .T. ) ;
#6836 = LINE ( 'NONE', #8172, #15641 ) ;
#6837 = UNCERTAINTY_MEASURE_WITH_UNIT (LENGTH_MEASURE( 1.000000000000000082E-05 ), #2473, 'distance_accuracy_value', 'NONE');
#6838 = ORIENTED_EDGE ( 'NONE', *, *, #17509, .F. ) ;
#6839 = AXIS2_PLACEMENT_3D ( 'NONE', #19964, #5968, #4421 ) ;
#6840 = CARTESIAN_POINT ( 'NONE',  ( 40.00000000000001421, -5.000000000000000888, -150.0000000000000000 ) ) ;
#6841 = ORIENTED_EDGE ( 'NONE', *, *, #8989, .F. ) ;
#6842 = UNCERTAINTY_MEASURE_WITH_UNIT (LENGTH_MEASURE( 1.000000000000000082E-05 ), #11983, 'distance_accuracy_value', 'NONE');
#6843 = FACE_OUTER_BOUND ( 'NONE', #14493, .T. ) ;
#6844 = CARTESIAN_POINT ( 'NONE',  ( 111.4893729001366012, 126.1646452518344859, 322.0399576098686225 ) ) ;
#6845 = UNCERTAINTY_MEASURE_WITH_UNIT (LENGTH_MEASURE( 1.000000000000000082E-05 ), #7124, 'distance_accuracy_value', 'NONE');
#6846 = ORIENTED_EDGE ( 'NONE', *, *, #18429, .T. ) ;
#6847 = EDGE_CURVE ( 'NONE', #12056, #63, #19829, .T. ) ;
#6848 = SURFACE_STYLE_FILL_AREA ( #8379 ) ;
#6849 = LINE ( 'NONE', #19073, #19225 ) ;
#6850 = CARTESIAN_POINT ( 'NONE',  ( 40.00000000000001421, 3.000000000000000888, -150.0000000000000000 ) ) ;
#6851 = CARTESIAN_POINT ( 'NONE',  ( 3.324999999999999734, 12.97499999999999964, 0.000000000000000000 ) ) ;
#6852 = CARTESIAN_POINT ( 'NONE',  ( 88.88953019741013861, 80.91625508013694912, 245.0000000000000000 ) ) ;
#6853 = CARTESIAN_POINT ( 'NONE',  ( 111.4893729001366012, 119.5973956464515879, 280.0825295754780768 ) ) ;
#6854 = EDGE_LOOP ( 'NONE', ( #1182, #1898, #8696, #2121 ) ) ;
#6855 = DIRECTION ( 'NONE',  ( -0.000000000000000000, -1.000000000000000000, 0.000000000000000000 ) ) ;
#6856 = CARTESIAN_POINT ( 'NONE',  ( 53.48937290013659407, 145.9162550801369491, 0.000000000000000000 ) ) ;
#6857 = VECTOR ( 'NONE', #8565, 1000.000000000000000 ) ;
#6858 = EDGE_CURVE ( 'NONE', #18127, #19519, #11925, .T. ) ;
#6859 = VECTOR ( 'NONE', #6484, 1000.000000000000000 ) ;
#6860 = VERTEX_POINT ( 'NONE', #19525 ) ;
#6861 = ADVANCED_FACE ( 'NONE', ( #2323 ), #18191, .T. ) ;
#6862 = ORIENTED_EDGE ( 'NONE', *, *, #2310, .T. ) ;
#6863 = DIRECTION ( 'NONE',  ( 0.000000000000000000, 0.000000000000000000, -1.000000000000000000 ) ) ;
#6864 = VERTEX_POINT ( 'NONE', #5845 ) ;
#6865 = UNCERTAINTY_MEASURE_WITH_UNIT (LENGTH_MEASURE( 1.000000000000000082E-05 ), #2202, 'distance_accuracy_value', 'NONE');
#6866 = CARTESIAN_POINT ( 'NONE',  ( -1.000000000000000888, 138.7545334744432637, 510.3921618609452935 ) ) ;
#6867 = CARTESIAN_POINT ( 'NONE',  ( 2.257948793614858118, 39.01519438325225053, 9.228844315538687226 ) ) ;
#6868 = VERTEX_POINT ( 'NONE', #17066 ) ;
#6869 = CARTESIAN_POINT ( 'NONE',  ( 463.8334540492693350, 191.8198460455371333, 81.76606011801540319 ) ) ;
#6870 = AXIS2_PLACEMENT_3D ( 'NONE', #16550, #659, #16367 ) ;
#6871 = EDGE_CURVE ( 'NONE', #3507, #9496, #3287, .T. ) ;
#6872 = CARTESIAN_POINT ( 'NONE',  ( -36.00000000000000000, 4.408728476930470856E-15, -135.0000000000000284 ) ) ;
#6873 = DIRECTION ( 'NONE',  ( 1.000000000000000000, -0.000000000000000000, -0.000000000000000000 ) ) ;
#6874 = DIRECTION ( 'NONE',  ( 0.000000000000000000, 0.000000000000000000, -1.000000000000000000 ) ) ;
#6875 = ORIENTED_EDGE ( 'NONE', *, *, #3627, .T. ) ;
#6876 = DIRECTION ( 'NONE',  ( 0.000000000000000000, 0.000000000000000000, 1.000000000000000000 ) ) ;
#6877 = DIRECTION ( 'NONE',  ( 0.000000000000000000, 1.000000000000000000, 0.000000000000000000 ) ) ;
#6878 = DIRECTION ( 'NONE',  ( -1.000000000000000000, -0.000000000000000000, -0.000000000000000000 ) ) ;
#6879 = CARTESIAN_POINT ( 'NONE',  ( 423.8334540492694487, 191.8198460455371333, 225.0057801310552463 ) ) ;
#6880 = DIRECTION ( 'NONE',  ( 0.000000000000000000, 0.000000000000000000, 1.000000000000000000 ) ) ;
#6881 = EDGE_CURVE ( 'NONE', #2165, #15076, #18609, .T. ) ;
#6882 = DIRECTION ( 'NONE',  ( -0.000000000000000000, -0.000000000000000000, 1.000000000000000000 ) ) ;
#6883 = VERTEX_POINT ( 'NONE', #13977 ) ;
#6884 = STYLED_ITEM ( 'NONE', ( #1579 ), #4658 ) ;
#6885 = EDGE_CURVE ( 'NONE', #15750, #17405, #14148, .T. ) ;
#6886 = ORIENTED_EDGE ( 'NONE', *, *, #13913, .F. ) ;
#6887 = EDGE_CURVE ( 'NONE', #15013, #10819, #18388, .T. ) ;
#6888 = ORIENTED_EDGE ( 'NONE', *, *, #14826, .T. ) ;
#6889 = LINE ( 'NONE', #13173, #9267 ) ;
#6890 = DIRECTION ( 'NONE',  ( 0.000000000000000000, 0.000000000000000000, 1.000000000000000000 ) ) ;
#6891 = VERTEX_POINT ( 'NONE', #1163 ) ;
#6892 = EDGE_CURVE ( 'NONE', #11867, #18810, #16802, .T. ) ;
#6893 = CARTESIAN_POINT ( 'NONE',  ( 53.48937290013659407, 0.000000000000000000, 0.000000000000000000 ) ) ;
#6894 = FILL_AREA_STYLE_COLOUR ( '', #7320 ) ;
#6895 = ADVANCED_FACE ( 'NONE', ( #13677 ), #4689, .T. ) ;
#6896 = ORIENTED_EDGE ( 'NONE', *, *, #14628, .T. ) ;
#6897 = CARTESIAN_POINT ( 'NONE',  ( 111.4893729001366012, 127.7247684487574304, 250.0000000000000000 ) ) ;
#6898 = DIRECTION ( 'NONE',  ( 0.000000000000000000, -0.000000000000000000, 1.000000000000000000 ) ) ;
#6899 = CARTESIAN_POINT ( 'NONE',  ( 0.7372031773519938103, 138.7723821178321657, 490.5025619606645364 ) ) ;
#6900 = STYLED_ITEM ( 'NONE', ( #11069 ), #4924 ) ;
#6901 = DIRECTION ( 'NONE',  ( 0.000000000000000000, 0.000000000000000000, 1.000000000000000000 ) ) ;
#6902 = AXIS2_PLACEMENT_3D ( 'NONE', #19699, #14780, #10057 ) ;
#6903 = CARTESIAN_POINT ( 'NONE',  ( 25.99999999999997868, 10.00000000000000000, -39.99999999999999289 ) ) ;
#6904 =( NAMED_UNIT ( * ) SI_UNIT ( $, .STERADIAN. ) SOLID_ANGLE_UNIT ( ) );
#6905 = FACE_BOUND ( 'NONE', #8194, .T. ) ;
#6906 = LINE ( 'NONE', #13487, #11169 ) ;
#6907 = CARTESIAN_POINT ( 'NONE',  ( 40.00000000000000000, 68.00000000000000000, 26.00000000000000355 ) ) ;
#6908 = CARTESIAN_POINT ( 'NONE',  ( 108.9893729001365870, 144.5787140289007766, 293.4524157190248275 ) ) ;
#6909 = ORIENTED_EDGE ( 'NONE', *, *, #12936, .F. ) ;
#6910 = EDGE_LOOP ( 'NONE', ( #13844, #18147, #8216, #3346 ) ) ;
#6911 = AXIS2_PLACEMENT_3D ( 'NONE', #3504, #8342, #18006 ) ;
#6912 = ORIENTED_EDGE ( 'NONE', *, *, #7945, .T. ) ;
#6913 = COLOUR_RGB ( '', 0.31764706, 0.68627451, 0.89019608) ;
#6914 = ORIENTED_EDGE ( 'NONE', *, *, #2184, .F. ) ;
#6915 = ORIENTED_EDGE ( 'NONE', *, *, #15928, .F. ) ;
#6916 = ADVANCED_FACE ( 'NONE', ( #16977 ), #20134, .T. ) ;
#6917 = DIRECTION ( 'NONE',  ( 1.000000000000000000, 5.889072920838430686E-16, -0.000000000000000000 ) ) ;
#6918 = DIRECTION ( 'NONE',  ( 0.000000000000000000, -0.7791332379872890623, -0.6268583551835633649 ) ) ;
#6919 = CYLINDRICAL_SURFACE ( 'NONE', #4954, 7.999999999999996447 ) ;
#6920 = EDGE_CURVE ( 'NONE', #6521, #10962, #17423, .T. ) ;
#6921 = CYLINDRICAL_SURFACE ( 'NONE', #1942, 10.00000000000000178 ) ;
#6922 = EDGE_CURVE ( 'NONE', #6498, #13953, #12434, .T. ) ;
#6923 = CARTESIAN_POINT ( 'NONE',  ( -15.00000000000000000, 317.7545334744432353, 495.1946179577816451 ) ) ;
#6924 = DIRECTION ( 'NONE',  ( 1.000000000000000000, 0.000000000000000000, 8.673617379884027583E-16 ) ) ;
#6925 = CARTESIAN_POINT ( 'NONE',  ( 0.000000000000000000, 26.00000000000000000, 0.000000000000000000 ) ) ;
#6926 = LINE ( 'NONE', #13312, #2200 ) ;
#6927 = COLOUR_RGB ( '', 0.72549020, 0.75294118, 0.79215686) ;
#6928 =( GEOMETRIC_REPRESENTATION_CONTEXT ( 3 ) GLOBAL_UNCERTAINTY_ASSIGNED_CONTEXT ( ( #15289 ) ) GLOBAL_UNIT_ASSIGNED_CONTEXT ( ( #4292, #2836, #12212 ) ) REPRESENTATION_CONTEXT ( 'NONE', 'WORKASPACE' ) );
#6929 = LINE ( 'NONE', #6723, #5304 ) ;
#6930 = DIRECTION ( 'NONE',  ( 0.000000000000000000, 1.000000000000000000, 0.000000000000000000 ) ) ;
#6931 = FILL_AREA_STYLE_COLOUR ( '', #5431 ) ;
#6932 = ORIENTED_EDGE ( 'NONE', *, *, #4090, .T. ) ;
#6933 = ORIENTED_EDGE ( 'NONE', *, *, #7388, .T. ) ;
#6934 = ORIENTED_EDGE ( 'NONE', *, *, #13545, .F. ) ;
#6935 = COLOUR_RGB ( '', 0.09019608, 0.27058824, 0.51372549) ;
#6936 = CIRCLE ( 'NONE', #19407, 0.5249999999999994671 ) ;
#6937 = ADVANCED_FACE ( 'NONE', ( #7583 ), #8921, .F. ) ;
#6938 = AXIS2_PLACEMENT_3D ( 'NONE', #1449, #3004, #9498 ) ;
#6939 = LINE ( 'NONE', #16631, #9558 ) ;
#6940 =( NAMED_UNIT ( * ) SI_UNIT ( $, .STERADIAN. ) SOLID_ANGLE_UNIT ( ) );
#6941 = FILL_AREA_STYLE_COLOUR ( '', #13830 ) ;
#6942 = ORIENTED_EDGE ( 'NONE', *, *, #6986, .F. ) ;
#6943 = DIRECTION ( 'NONE',  ( -0.000000000000000000, -1.000000000000000000, -0.000000000000000000 ) ) ;
#6944 = DIRECTION ( 'NONE',  ( 0.000000000000000000, -1.000000000000000000, 0.000000000000000000 ) ) ;
#6945 = DIRECTION ( 'NONE',  ( 0.000000000000000000, 0.000000000000000000, -1.000000000000000000 ) ) ;
#6946 = PLANE ( 'NONE',  #7662 ) ;
#6947 = CYLINDRICAL_SURFACE ( 'NONE', #5301, 10.00000000000000888 ) ;
#6948 = CARTESIAN_POINT ( 'NONE',  ( -37.00000000000000711, 10.00000000000000000, 23.00000000000000000 ) ) ;
#6949 = EDGE_LOOP ( 'NONE', ( #17790, #227, #4378, #13234 ) ) ;
#6950 = CARTESIAN_POINT ( 'NONE',  ( -31.00000000000005329, 10.00000000000000000, -26.00000000000000355 ) ) ;
#6951 = DIRECTION ( 'NONE',  ( 0.000000000000000000, 0.000000000000000000, -1.000000000000000000 ) ) ;
#6952 = FACE_OUTER_BOUND ( 'NONE', #7953, .T. ) ;
#6953 = AXIS2_PLACEMENT_3D ( 'NONE', #863, #18283, #8816 ) ;
#6954 = VECTOR ( 'NONE', #18130, 1000.000000000000000 ) ;
#6955 = ORIENTED_EDGE ( 'NONE', *, *, #4971, .T. ) ;
#6956 = EDGE_LOOP ( 'NONE', ( #4829, #1238, #4587, #16771 ) ) ;
#6957 = CARTESIAN_POINT ( 'NONE',  ( -81.18192946989275072, 140.4048636633015406, 499.8237260975782874 ) ) ;
#6958 = VERTEX_POINT ( 'NONE', #10777 ) ;
#6959 = AXIS2_PLACEMENT_3D ( 'NONE', #3392, #9465, #1718 ) ;
#6960 = CARTESIAN_POINT ( 'NONE',  ( 0.1972064085032624869, 38.00000000000002132, 9.500000000000005329 ) ) ;
#6961 = VERTEX_POINT ( 'NONE', #15535 ) ;
#6962 = AXIS2_PLACEMENT_3D ( 'NONE', #1845, #205, #8156 ) ;
#6963 = DIRECTION ( 'NONE',  ( 0.000000000000000000, 1.000000000000000000, -0.000000000000000000 ) ) ;
#6964 = DIRECTION ( 'NONE',  ( -0.000000000000000000, -1.000000000000000000, -0.000000000000000000 ) ) ;
#6965 = DIRECTION ( 'NONE',  ( 1.000000000000000000, 5.889072920838430686E-16, 0.000000000000000000 ) ) ;
#6966 =( NAMED_UNIT ( * ) PLANE_ANGLE_UNIT ( ) SI_UNIT ( $, .RADIAN. ) );
#6967 = VERTEX_POINT ( 'NONE', #2929 ) ;
#6968 = LINE ( 'NONE', #460, #268 ) ;
#6969 = CARTESIAN_POINT ( 'NONE',  ( -26.00000000000001776, 0.000000000000000000, 31.00000000000003553 ) ) ;
#6970 = LINE ( 'NONE', #13254, #4034 ) ;
#6971 = CARTESIAN_POINT ( 'NONE',  ( 0.000000000000000000, 38.00000000000000711, -5.741599279633704455E-16 ) ) ;
#6972 = CARTESIAN_POINT ( 'NONE',  ( 0.000000000000000000, 0.000000000000000000, 0.000000000000000000 ) ) ;
#6973 = ORIENTED_EDGE ( 'NONE', *, *, #19683, .F. ) ;
#6974 = LINE ( 'NONE', #17578, #14860 ) ;
#6975 = EDGE_CURVE ( 'NONE', #5387, #14439, #5931, .T. ) ;
#6976 = VERTEX_POINT ( 'NONE', #11086 ) ;
#6977 = VECTOR ( 'NONE', #5324, 1000.000000000000000 ) ;
#6978 =( GEOMETRIC_REPRESENTATION_CONTEXT ( 3 ) GLOBAL_UNCERTAINTY_ASSIGNED_CONTEXT ( ( #14324 ) ) GLOBAL_UNIT_ASSIGNED_CONTEXT ( ( #19246, #15978, #17887 ) ) REPRESENTATION_CONTEXT ( 'NONE', 'WORKASPACE' ) );
#6979 = EDGE_LOOP ( 'NONE', ( #3531, #14469, #2589, #12524, #18649, #6426, #3707, #8641, #5840, #7183, #12520, #9488, #4870, #4712, #388, #11922, #9119, #1297, #11432, #15575, #18317, #20238, #18672, #4657, #15007, #11009, #2796, #18290 ) ) ;
#6980 = ORIENTED_EDGE ( 'NONE', *, *, #16821, .F. ) ;
#6981 = ORIENTED_EDGE ( 'NONE', *, *, #15457, .T. ) ;
#6982 = DIRECTION ( 'NONE',  ( -0.000000000000000000, 1.000000000000000000, -0.000000000000000000 ) ) ;
#6983 = DIRECTION ( 'NONE',  ( 0.000000000000000000, 0.000000000000000000, 1.000000000000000000 ) ) ;
#6984 = ORIENTED_EDGE ( 'NONE', *, *, #16087, .T. ) ;
#6985 =( LENGTH_UNIT ( ) NAMED_UNIT ( * ) SI_UNIT ( .MILLI., .METRE. ) );
#6986 = EDGE_CURVE ( 'NONE', #7735, #15475, #3157, .T. ) ;
#6987 = CARTESIAN_POINT ( 'NONE',  ( 2.181929469892510465, 138.7545334744432637, 490.5655098179832976 ) ) ;
#6988 = DIRECTION ( 'NONE',  ( -3.854941057726249437E-16, -0.000000000000000000, 1.000000000000000000 ) ) ;
#6989 = VECTOR ( 'NONE', #6235, 1000.000000000000000 ) ;
#6990 = CARTESIAN_POINT ( 'NONE',  ( -40.00000000000000711, 10.00000000000000000, 26.00000000000000000 ) ) ;
#6991 = LINE ( 'NONE', #10381, #11688 ) ;
#6992 = DIRECTION ( 'NONE',  ( 1.000000000000000000, -0.000000000000000000, -0.000000000000000000 ) ) ;
#6993 = ADVANCED_FACE ( 'NONE', ( #6555 ), #4901, .F. ) ;
#6994 = PRESENTATION_LAYER_ASSIGNMENT (  '', '', ( #19147 ) ) ;
#6995 = CARTESIAN_POINT ( 'NONE',  ( 78.48937290013660117, 113.1299228374914208, 220.6387154965113382 ) ) ;
#6996 =( LENGTH_UNIT ( ) NAMED_UNIT ( * ) SI_UNIT ( .MILLI., .METRE. ) );
#6997 = EDGE_CURVE ( 'NONE', #7067, #12183, #3250, .T. ) ;
#6998 = DIRECTION ( 'NONE',  ( -0.000000000000000000, 1.000000000000000000, -0.000000000000000000 ) ) ;
#6999 = CARTESIAN_POINT ( 'NONE',  ( 53.48937290013660117, 77.72476844875745883, 252.0000000000000000 ) ) ;
#7000 = ORIENTED_EDGE ( 'NONE', *, *, #17509, .T. ) ;
#7001 = CIRCLE ( 'NONE', #9288, 4.999999999999997335 ) ;
#7002 = LINE ( 'NONE', #594, #19120 ) ;
#7003 = DIRECTION ( 'NONE',  ( 1.000000000000000000, 0.000000000000000000, 0.000000000000000000 ) ) ;
#7004 = ORIENTED_EDGE ( 'NONE', *, *, #6871, .F. ) ;
#7005 = EDGE_CURVE ( 'NONE', #19679, #19612, #6936, .T. ) ;
#7006 = EDGE_CURVE ( 'NONE', #14093, #3271, #1792, .T. ) ;
#7007 = ORIENTED_EDGE ( 'NONE', *, *, #10375, .T. ) ;
#7008 = MECHANICAL_DESIGN_GEOMETRIC_PRESENTATION_REPRESENTATION (  '', ( #15894 ), #18166 ) ;
#7009 = CIRCLE ( 'NONE', #708, 10.00000000000000888 ) ;
#7010 = UNCERTAINTY_MEASURE_WITH_UNIT (LENGTH_MEASURE( 1.000000000000000082E-05 ), #11834, 'distance_accuracy_value', 'NONE');
#7011 = ORIENTED_EDGE ( 'NONE', *, *, #4462, .F. ) ;
#7012 = MECHANICAL_DESIGN_GEOMETRIC_PRESENTATION_REPRESENTATION (  '', ( #5373 ), #6006 ) ;
#7013 = VERTEX_POINT ( 'NONE', #19106 ) ;
#7014 = ORIENTED_EDGE ( 'NONE', *, *, #13666, .F. ) ;
#7015 =( NAMED_UNIT ( * ) SI_UNIT ( $, .STERADIAN. ) SOLID_ANGLE_UNIT ( ) );
#7016 = DIRECTION ( 'NONE',  ( 0.000000000000000000, 0.000000000000000000, -1.000000000000000000 ) ) ;
#7017 = EDGE_CURVE ( 'NONE', #7147, #10363, #12844, .T. ) ;
#7018 = CARTESIAN_POINT ( 'NONE',  ( 26.00000000000000355, 19.00000000000000000, -31.00000000000003908 ) ) ;
#7019 = VECTOR ( 'NONE', #11570, 1000.000000000000000 ) ;
#7020 = LINE ( 'NONE', #4011, #2730 ) ;
#7021 = CARTESIAN_POINT ( 'NONE',  ( 458.8334540492693350, 191.8198460455371333, 158.2339398819845826 ) ) ;
#7022 = VECTOR ( 'NONE', #13337, 1000.000000000000000 ) ;
#7023 = MECHANICAL_DESIGN_GEOMETRIC_PRESENTATION_REPRESENTATION (  '', ( #15905 ), #7332 ) ;
#7024 = DIRECTION ( 'NONE',  ( 0.000000000000000000, 0.000000000000000000, 1.000000000000000000 ) ) ;
#7025 = ADVANCED_FACE ( 'NONE', ( #18015 ), #8851, .F. ) ;
#7026 = LINE ( 'NONE', #18024, #5953 ) ;
#7027 = AXIS2_PLACEMENT_3D ( 'NONE', #16446, #18060, #2290 ) ;
#7028 =( LENGTH_UNIT ( ) NAMED_UNIT ( * ) SI_UNIT ( .MILLI., .METRE. ) );
#7029 = CARTESIAN_POINT ( 'NONE',  ( -23.00000000000002132, 10.00000000000000000, 31.00000000000003553 ) ) ;
#7030 = EDGE_CURVE ( 'NONE', #6860, #10847, #10290, .T. ) ;
#7031 = VECTOR ( 'NONE', #7217, 1000.000000000000000 ) ;
#7032 = ORIENTED_EDGE ( 'NONE', *, *, #19762, .F. ) ;
#7033 = ORIENTED_EDGE ( 'NONE', *, *, #5591, .F. ) ;
#7034 = CARTESIAN_POINT ( 'NONE',  ( 21.00000000000000000, 19.00000000000000000, -31.00000000000003908 ) ) ;
#7035 = UNCERTAINTY_MEASURE_WITH_UNIT (LENGTH_MEASURE( 1.000000000000000082E-05 ), #18526, 'distance_accuracy_value', 'NONE');
#7036 = EDGE_LOOP ( 'NONE', ( #2750, #19596, #3028, #12682 ) ) ;
#7037 = VECTOR ( 'NONE', #17631, 1000.000000000000000 ) ;
#7038 = AXIS2_PLACEMENT_3D ( 'NONE', #20143, #13770, #20259 ) ;
#7039 = ORIENTED_EDGE ( 'NONE', *, *, #19791, .T. ) ;
#7040 =( NAMED_UNIT ( * ) PLANE_ANGLE_UNIT ( ) SI_UNIT ( $, .RADIAN. ) );
#7041 = CARTESIAN_POINT ( 'NONE',  ( 111.4893729001366012, 129.7247684487574588, 283.6050404526570219 ) ) ;
#7042 = UNCERTAINTY_MEASURE_WITH_UNIT (LENGTH_MEASURE( 1.000000000000000082E-05 ), #15339, 'distance_accuracy_value', 'NONE');
#7043 = PRESENTATION_STYLE_ASSIGNMENT (( #2488 ) ) ;
#7044 = ORIENTED_EDGE ( 'NONE', *, *, #2369, .F. ) ;
#7045 = SURFACE_STYLE_USAGE ( .BOTH. , #17340 ) ;
#7046 = CARTESIAN_POINT ( 'NONE',  ( 25.99999999999998224, 8.000000000000000000, -32.99999999999999289 ) ) ;
#7047 = CARTESIAN_POINT ( 'NONE',  ( 1.000000000001310063, 216.7545334744432921, 489.5655098179835818 ) ) ;
#7048 = AXIS2_PLACEMENT_3D ( 'NONE', #19769, #3927, #11270 ) ;
#7049 = EDGE_CURVE ( 'NONE', #9009, #9433, #8644, .T. ) ;
#7050 = DIRECTION ( 'NONE',  ( 0.000000000000000000, 0.000000000000000000, 1.000000000000000000 ) ) ;
#7051 = DIRECTION ( 'NONE',  ( 1.000000000000000000, -0.000000000000000000, 0.000000000000000000 ) ) ;
#7052 = VERTEX_POINT ( 'NONE', #698 ) ;
#7053 = DIRECTION ( 'NONE',  ( -1.000000000000000000, -0.000000000000000000, -0.000000000000000000 ) ) ;
#7054 = AXIS2_PLACEMENT_3D ( 'NONE', #5153, #19258, #5040 ) ;
#7055 = COLOUR_RGB ( '', 0.31764706, 0.68627451, 0.89019608) ;
#7056 = VECTOR ( 'NONE', #14426, 1000.000000000000000 ) ;
#7057 = VECTOR ( 'NONE', #6527, 1000.000000000000000 ) ;
#7058 = ORIENTED_EDGE ( 'NONE', *, *, #19672, .T. ) ;
#7059 = ORIENTED_EDGE ( 'NONE', *, *, #16790, .F. ) ;
#7060 =( GEOMETRIC_REPRESENTATION_CONTEXT ( 3 ) GLOBAL_UNCERTAINTY_ASSIGNED_CONTEXT ( ( #16447 ) ) GLOBAL_UNIT_ASSIGNED_CONTEXT ( ( #8201, #18789, #5115 ) ) REPRESENTATION_CONTEXT ( 'NONE', 'WORKASPACE' ) );
#7061 = VERTEX_POINT ( 'NONE', #13303 ) ;
#7062 = DIRECTION ( 'NONE',  ( 0.000000000000000000, 0.000000000000000000, 1.000000000000000000 ) ) ;
#7063 =( GEOMETRIC_REPRESENTATION_CONTEXT ( 3 ) GLOBAL_UNCERTAINTY_ASSIGNED_CONTEXT ( ( #10519 ) ) GLOBAL_UNIT_ASSIGNED_CONTEXT ( ( #8571, #12935, #19197 ) ) REPRESENTATION_CONTEXT ( 'NONE', 'WORKASPACE' ) );
#7064 = CARTESIAN_POINT ( 'NONE',  ( 463.8334540492693350, 191.8198460455371333, 81.76606011801540319 ) ) ;
#7065 = UNCERTAINTY_MEASURE_WITH_UNIT (LENGTH_MEASURE( 1.000000000000000082E-05 ), #17402, 'distance_accuracy_value', 'NONE');
#7066 = VECTOR ( 'NONE', #4651, 1000.000000000000000 ) ;
#7067 = VERTEX_POINT ( 'NONE', #3819 ) ;
#7068 = CARTESIAN_POINT ( 'NONE',  ( 5.425003271131650706, -12.64814671169700055, 1.549064719741994274E-15 ) ) ;
#7069 =( LENGTH_UNIT ( ) NAMED_UNIT ( * ) SI_UNIT ( .MILLI., .METRE. ) );
#7070 = MECHANICAL_DESIGN_GEOMETRIC_PRESENTATION_REPRESENTATION (  '', ( #1093 ), #5415 ) ;
#7071 = CARTESIAN_POINT ( 'NONE',  ( 463.8334540492693918, 167.8734308960555950, 250.0000000000000000 ) ) ;
#7072 = CARTESIAN_POINT ( 'NONE',  ( 423.8334540492694487, 191.8198460455371333, 71.76606011801538898 ) ) ;
#7073 = ORIENTED_EDGE ( 'NONE', *, *, #17916, .F. ) ;
#7074 = CYLINDRICAL_SURFACE ( 'NONE', #18694, 2.999999999999999112 ) ;
#7075 = DIRECTION ( 'NONE',  ( 0.000000000000000000, 0.000000000000000000, -1.000000000000000000 ) ) ;
#7076 = FACE_BOUND ( 'NONE', #1724, .T. ) ;
#7077 = LINE ( 'NONE', #13255, #11641 ) ;
#7078 = VECTOR ( 'NONE', #10444, 1000.000000000000000 ) ;
#7079 = EDGE_CURVE ( 'NONE', #20011, #19900, #4628, .T. ) ;
#7080 =( NAMED_UNIT ( * ) SI_UNIT ( $, .STERADIAN. ) SOLID_ANGLE_UNIT ( ) );
#7081 = CIRCLE ( 'NONE', #13662, 10.00000000000000888 ) ;
#7082 = ORIENTED_EDGE ( 'NONE', *, *, #1287, .T. ) ;
#7083 = CIRCLE ( 'NONE', #18893, 10.00000000000000888 ) ;
#7084 = ORIENTED_EDGE ( 'NONE', *, *, #13423, .T. ) ;
#7085 = CIRCLE ( 'NONE', #17921, 0.9999999999999974465 ) ;
#7086 = ORIENTED_EDGE ( 'NONE', *, *, #317, .F. ) ;
#7087 = VECTOR ( 'NONE', #15057, 1000.000000000000000 ) ;
#7088 = AXIS2_PLACEMENT_3D ( 'NONE', #5737, #2629, #2733 ) ;
#7089 = ORIENTED_EDGE ( 'NONE', *, *, #15974, .F. ) ;
#7090 = ORIENTED_EDGE ( 'NONE', *, *, #14342, .F. ) ;
#7091 = FACE_OUTER_BOUND ( 'NONE', #6036, .T. ) ;
#7092 = LINE ( 'NONE', #2531, #2525 ) ;
#7093 = VECTOR ( 'NONE', #18729, 1000.000000000000000 ) ;
#7094 = ORIENTED_EDGE ( 'NONE', *, *, #15439, .T. ) ;
#7095 = LINE ( 'NONE', #3682, #2448 ) ;
#7096 = DIRECTION ( 'NONE',  ( 1.000000000000000000, 0.000000000000000000, 0.000000000000000000 ) ) ;
#7097 = EDGE_CURVE ( 'NONE', #3610, #15515, #8555, .T. ) ;
#7098 = VECTOR ( 'NONE', #14759, 1000.000000000000000 ) ;
#7099 = PRESENTATION_STYLE_ASSIGNMENT (( #19628 ) ) ;
#7100 = CIRCLE ( 'NONE', #16652, 4.999999999999997335 ) ;
#7101 = PLANE ( 'NONE',  #11258 ) ;
#7102 = CARTESIAN_POINT ( 'NONE',  ( -0.5185395424450671698, 138.8549385558393681, 489.7242651416971739 ) ) ;
#7103 =( GEOMETRIC_REPRESENTATION_CONTEXT ( 3 ) GLOBAL_UNCERTAINTY_ASSIGNED_CONTEXT ( ( #17945 ) ) GLOBAL_UNIT_ASSIGNED_CONTEXT ( ( #7797, #4903, #15952 ) ) REPRESENTATION_CONTEXT ( 'NONE', 'WORKASPACE' ) );
#7104 = CYLINDRICAL_SURFACE ( 'NONE', #4869, 1.000000000000000888 ) ;
#7105 = CARTESIAN_POINT ( 'NONE',  ( -58.16843972078500258, 317.7545334744432353, 489.0536462814662286 ) ) ;
#7106 = CARTESIAN_POINT ( 'NONE',  ( 458.8334540492693350, 0.000000000000000000, 0.000000000000000000 ) ) ;
#7107 = SURFACE_SIDE_STYLE ('',( #788 ) ) ;
#7108 = UNCERTAINTY_MEASURE_WITH_UNIT (LENGTH_MEASURE( 1.000000000000000082E-05 ), #13008, 'distance_accuracy_value', 'NONE');
#7109 = CYLINDRICAL_SURFACE ( 'NONE', #5963, 3.299999999999997158 ) ;
#7110 = CARTESIAN_POINT ( 'NONE',  ( -211.5106270998635409, 113.1299228374912502, 79.58252780074349175 ) ) ;
#7111 = ORIENTED_EDGE ( 'NONE', *, *, #10734, .F. ) ;
#7112 = VECTOR ( 'NONE', #4284, 1000.000000000000000 ) ;
#7113 = EDGE_CURVE ( 'NONE', #9509, #15515, #15138, .T. ) ;
#7114 =( REPRESENTATION_RELATIONSHIP ('NONE','NONE', #12483, #13279 ) REPRESENTATION_RELATIONSHIP_WITH_TRANSFORMATION ( #2912 )SHAPE_REPRESENTATION_RELATIONSHIP( ) );
#7115 = ORIENTED_EDGE ( 'NONE', *, *, #6892, .T. ) ;
#7116 = EDGE_CURVE ( 'NONE', #995, #4612, #9544, .T. ) ;
#7117 = VERTEX_POINT ( 'NONE', #10100 ) ;
#7118 = AXIS2_PLACEMENT_3D ( 'NONE', #13227, #18247, #19473 ) ;
#7119 = FACE_OUTER_BOUND ( 'NONE', #19119, .T. ) ;
#7120 = CARTESIAN_POINT ( 'NONE',  ( -21.85283368562565443, 319.7545334744432353, 481.2863735482146694 ) ) ;
#7121 = CARTESIAN_POINT ( 'NONE',  ( 463.8334540492693350, 214.2156642432025251, 250.0000000000000000 ) ) ;
#7122 = CIRCLE ( 'NONE', #5156, 12.64814671169700055 ) ;
#7123 = EDGE_CURVE ( 'NONE', #13692, #6152, #4223, .T. ) ;
#7124 =( LENGTH_UNIT ( ) NAMED_UNIT ( * ) SI_UNIT ( .MILLI., .METRE. ) );
#7125 = CARTESIAN_POINT ( 'NONE',  ( -78.99999999999995737, 138.3494706343262237, 489.1604469778678776 ) ) ;
#7126 = DIRECTION ( 'NONE',  ( 1.000000000000000000, 0.000000000000000000, 0.000000000000000000 ) ) ;
#7127 = SURFACE_STYLE_FILL_AREA ( #15249 ) ;
#7128 = DIRECTION ( 'NONE',  ( 1.000000000000000000, 0.000000000000000000, -0.000000000000000000 ) ) ;
#7129 = EDGE_CURVE ( 'NONE', #530, #10363, #11638, .T. ) ;
#7130 = PLANE ( 'NONE',  #13517 ) ;
#7131 = CARTESIAN_POINT ( 'NONE',  ( 0.000000000000000000, 145.9162550801369491, -97.94896630388704750 ) ) ;
#7132 = CARTESIAN_POINT ( 'NONE',  ( -26.00000000000001776, 10.00000000000000000, 33.00000000000000711 ) ) ;
#7133 = CARTESIAN_POINT ( 'NONE',  ( 2.181929469892549545, 147.7545334744432921, 491.0690926367355473 ) ) ;
#7134 = DIRECTION ( 'NONE',  ( -1.000000000000000000, 0.000000000000000000, -0.000000000000000000 ) ) ;
#7135 = VECTOR ( 'NONE', #19358, 1000.000000000000000 ) ;
#7136 = ADVANCED_FACE ( 'NONE', ( #2346 ), #6919, .T. ) ;
#7137 = ORIENTED_EDGE ( 'NONE', *, *, #12163, .T. ) ;
#7138 = VECTOR ( 'NONE', #1499, 1000.000000000000000 ) ;
#7139 = VERTEX_POINT ( 'NONE', #7213 ) ;
#7140 = VERTEX_POINT ( 'NONE', #2553 ) ;
#7141 = ORIENTED_EDGE ( 'NONE', *, *, #7859, .F. ) ;
#7142 = EDGE_CURVE ( 'NONE', #19389, #7675, #15494, .T. ) ;
#7143 = VERTEX_POINT ( 'NONE', #803 ) ;
#7144 = CARTESIAN_POINT ( 'NONE',  ( 0.000000000000000000, 0.000000000000000000, 0.000000000000000000 ) ) ;
#7145 =( LENGTH_UNIT ( ) NAMED_UNIT ( * ) SI_UNIT ( .MILLI., .METRE. ) );
#7146 = DIRECTION ( 'NONE',  ( 0.000000000000000000, 0.000000000000000000, -1.000000000000000000 ) ) ;
#7147 = VERTEX_POINT ( 'NONE', #14825 ) ;
#7148 = ADVANCED_FACE ( 'NONE', ( #7119 ), #13410, .F. ) ;
#7149 = DIRECTION ( 'NONE',  ( 1.000000000000000000, 0.000000000000000000, 1.322948291343119651E-12 ) ) ;
#7150 = DIRECTION ( 'NONE',  ( 1.445602896647347002E-15, 0.000000000000000000, 1.000000000000000000 ) ) ;
#7151 = CARTESIAN_POINT ( 'NONE',  ( 1.750000000000000000, 14.59999999999999964, 0.000000000000000000 ) ) ;
#7152 = EDGE_CURVE ( 'NONE', #6221, #6137, #19737, .T. ) ;
#7153 = FACE_OUTER_BOUND ( 'NONE', #6149, .T. ) ;
#7154 = VECTOR ( 'NONE', #5332, 1000.000000000000000 ) ;
#7155 = CARTESIAN_POINT ( 'NONE',  ( -79.99999999999995737, 138.7545334744432637, 477.3411705753777596 ) ) ;
#7156 =( LENGTH_UNIT ( ) NAMED_UNIT ( * ) SI_UNIT ( .MILLI., .METRE. ) );
#7157 = DIRECTION ( 'NONE',  ( -6.120180426682197225E-17, 0.6235460666509320404, -0.7817866094812263578 ) ) ;
#7158 =( NAMED_UNIT ( * ) PLANE_ANGLE_UNIT ( ) SI_UNIT ( $, .RADIAN. ) );
#7159 = ORIENTED_EDGE ( 'NONE', *, *, #5503, .T. ) ;
#7160 =( LENGTH_UNIT ( ) NAMED_UNIT ( * ) SI_UNIT ( .MILLI., .METRE. ) );
#7161 = DIRECTION ( 'NONE',  ( 0.000000000000000000, 0.000000000000000000, -1.000000000000000000 ) ) ;
#7162 = CARTESIAN_POINT ( 'NONE',  ( 0.000000000000000000, 0.000000000000000000, 0.000000000000000000 ) ) ;
#7163 = ORIENTED_EDGE ( 'NONE', *, *, #15524, .T. ) ;
#7164 = EDGE_LOOP ( 'NONE', ( #8889, #4539, #16266, #6744, #19285, #3973, #12623, #14680, #16813, #16967, #5674, #10021, #12357, #909, #15831, #18318, #5863, #692, #13885, #1049, #14254, #4375, #2852, #7554, #15936, #7159, #16749, #16537 ) ) ;
#7165 = ORIENTED_EDGE ( 'NONE', *, *, #11486, .F. ) ;
#7166 = ADVANCED_FACE ( 'NONE', ( #18107 ), #18217, .F. ) ;
#7167 = CARTESIAN_POINT ( 'NONE',  ( -79.99999999999995737, 316.7545334744432353, 495.1946179577816451 ) ) ;
#7168 = CYLINDRICAL_SURFACE ( 'NONE', #17424, 2.999999999999999556 ) ;
#7169 = ORIENTED_EDGE ( 'NONE', *, *, #2694, .F. ) ;
#7170 = FACE_OUTER_BOUND ( 'NONE', #10560, .T. ) ;
#7171 = CARTESIAN_POINT ( 'NONE',  ( -78.99999999999995737, 140.6767260202136072, 502.2320488918456931 ) ) ;
#7172 = DIRECTION ( 'NONE',  ( 1.000000000000000000, 0.000000000000000000, -0.000000000000000000 ) ) ;
#7173 = ADVANCED_FACE ( 'NONE', ( #15042 ), #11949, .F. ) ;
#7174 = UNCERTAINTY_MEASURE_WITH_UNIT (LENGTH_MEASURE( 1.000000000000000082E-05 ), #12636, 'distance_accuracy_value', 'NONE');
#7175 = CARTESIAN_POINT ( 'NONE',  ( -211.5106270998635409, 113.1299228374912502, 220.6387154965113382 ) ) ;
#7176 = FACE_OUTER_BOUND ( 'NONE', #15559, .T. ) ;
#7177 = SURFACE_STYLE_FILL_AREA ( #19913 ) ;
#7178 = AXIS2_PLACEMENT_3D ( 'NONE', #15363, #12150, #1192 ) ;
#7179 = ORIENTED_EDGE ( 'NONE', *, *, #8122, .T. ) ;
#7180 = DIRECTION ( 'NONE',  ( 6.123031769111888756E-17, -1.000000000000000000, -3.749151804555344967E-33 ) ) ;
#7181 = FACE_BOUND ( 'NONE', #19333, .T. ) ;
#7182 = EDGE_LOOP ( 'NONE', ( #13108, #7464, #1081, #19792, #5167, #2916, #7668, #15582 ) ) ;
#7183 = ORIENTED_EDGE ( 'NONE', *, *, #1528, .F. ) ;
#7184 = ORIENTED_EDGE ( 'NONE', *, *, #5484, .F. ) ;
#7185 = VECTOR ( 'NONE', #9229, 1000.000000000000000 ) ;
#7186 = ORIENTED_EDGE ( 'NONE', *, *, #7255, .T. ) ;
#7187 = DIRECTION ( 'NONE',  ( 0.000000000000000000, -0.000000000000000000, -1.000000000000000000 ) ) ;
#7188 = DIRECTION ( 'NONE',  ( 0.000000000000000000, 0.000000000000000000, 1.000000000000000000 ) ) ;
#7189 = ORIENTED_EDGE ( 'NONE', *, *, #196, .F. ) ;
#7190 = CARTESIAN_POINT ( 'NONE',  ( -20.99999999999999645, 8.000000000000000000, 35.00000000000001421 ) ) ;
#7191 = ADVANCED_FACE ( 'NONE', ( #982, #15354 ), #4805, .T. ) ;
#7192 = SURFACE_SIDE_STYLE ('',( #18300 ) ) ;
#7193 = DIRECTION ( 'NONE',  ( 0.000000000000000000, 0.000000000000000000, 1.000000000000000000 ) ) ;
#7194 = LINE ( 'NONE', #16474, #3369 ) ;
#7195 = CARTESIAN_POINT ( 'NONE',  ( -58.16843972078500258, 319.7545334744432353, 489.0536462814662286 ) ) ;
#7196 = CARTESIAN_POINT ( 'NONE',  ( 53.48937290013662249, 49.66333933884487806, 252.0000000000000000 ) ) ;
#7197 = LINE ( 'NONE', #19633, #19488 ) ;
#7198 = DIRECTION ( 'NONE',  ( -0.000000000000000000, -0.000000000000000000, 1.000000000000000000 ) ) ;
#7199 = SURFACE_STYLE_FILL_AREA ( #5751 ) ;
#7200 = FACE_OUTER_BOUND ( 'NONE', #13755, .T. ) ;
#7201 = FACE_BOUND ( 'NONE', #3684, .T. ) ;
#7202 = AXIS2_PLACEMENT_3D ( 'NONE', #15651, #3162, #9442 ) ;
#7203 = DIRECTION ( 'NONE',  ( 0.000000000000000000, 1.000000000000000000, -0.000000000000000000 ) ) ;
#7204 = LINE ( 'NONE', #5646, #10841 ) ;
#7205 = VERTEX_POINT ( 'NONE', #9058 ) ;
#7206 = VERTEX_POINT ( 'NONE', #1788 ) ;
#7207 = PRODUCT_DEFINITION_CONTEXT ( 'detailed design', #18669, 'design' ) ;
#7208 = EDGE_CURVE ( 'NONE', #14262, #14090, #7420, .T. ) ;
#7209 = ORIENTED_EDGE ( 'NONE', *, *, #11771, .F. ) ;
#7210 = ORIENTED_EDGE ( 'NONE', *, *, #6471, .T. ) ;
#7211 = FILL_AREA_STYLE_COLOUR ( '', #13396 ) ;
#7212 = DIRECTION ( 'NONE',  ( 0.000000000000000000, 0.000000000000000000, -1.000000000000000000 ) ) ;
#7213 = CARTESIAN_POINT ( 'NONE',  ( -19.00000000000001776, 8.000000000000000000, 36.00000000000000711 ) ) ;
#7214 = VECTOR ( 'NONE', #1965, 1000.000000000000000 ) ;
#7215 = LINE ( 'NONE', #5774, #13308 ) ;
#7216 = DIRECTION ( 'NONE',  ( -0.000000000000000000, -1.000000000000000000, 0.000000000000000000 ) ) ;
#7217 = DIRECTION ( 'NONE',  ( 1.000000000000000000, 5.889072920838430686E-16, -0.000000000000000000 ) ) ;
#7218 = EDGE_CURVE ( 'NONE', #19306, #18726, #9895, .T. ) ;
#7219 = CARTESIAN_POINT ( 'NONE',  ( 6.649999999999999467, 18.17500000000000071, 0.000000000000000000 ) ) ;
#7220 = LINE ( 'NONE', #12929, #20163 ) ;
#7221 = SURFACE_STYLE_USAGE ( .BOTH. , #4423 ) ;
#7222 = CARTESIAN_POINT ( 'NONE',  ( 1.163414459189985485E-15, 66.00000000000000000, 9.500000000000000000 ) ) ;
#7223 = CARTESIAN_POINT ( 'NONE',  ( -31.00000000000003197, 68.00000000000000000, -22.99999999999999645 ) ) ;
#7224 = FACE_OUTER_BOUND ( 'NONE', #6854, .T. ) ;
#7225 = AXIS2_PLACEMENT_3D ( 'NONE', #18443, #17320, #13918 ) ;
#7226 = VECTOR ( 'NONE', #4554, 1000.000000000000000 ) ;
#7227 = EDGE_CURVE ( 'NONE', #7485, #15108, #6287, .T. ) ;
#7228 = ORIENTED_EDGE ( 'NONE', *, *, #11522, .F. ) ;
#7229 = ORIENTED_EDGE ( 'NONE', *, *, #2310, .F. ) ;
#7230 = CARTESIAN_POINT ( 'NONE',  ( -1.994931997373328159E-14, 147.7545334744432921, 496.6642397995874489 ) ) ;
#7231 = ORIENTED_EDGE ( 'NONE', *, *, #16090, .T. ) ;
#7232 = ORIENTED_EDGE ( 'NONE', *, *, #12996, .F. ) ;
#7233 = SURFACE_STYLE_FILL_AREA ( #717 ) ;
#7234 = CARTESIAN_POINT ( 'NONE',  ( -25.99999999999999645, 0.000000000000000000, 31.00000000000003908 ) ) ;
#7235 = SURFACE_STYLE_FILL_AREA ( #3931 ) ;
#7236 = PRESENTATION_LAYER_ASSIGNMENT (  '', '', ( #5905 ) ) ;
#7237 =( LENGTH_UNIT ( ) NAMED_UNIT ( * ) SI_UNIT ( .MILLI., .METRE. ) );
#7238 = ADVANCED_FACE ( 'NONE', ( #18515 ), #6349, .F. ) ;
#7239 = FILL_AREA_STYLE ('',( #2682 ) ) ;
#7241 = EDGE_CURVE ( 'NONE', #14656, #13534, #14832, .T. ) ;
#7240 = LINE ( 'NONE', #4342, #13268 ) ;
#7242 = AXIS2_PLACEMENT_3D ( 'NONE', #591, #5344, #3899 ) ;
#7243 = DIRECTION ( 'NONE',  ( -0.000000000000000000, -1.000000000000000000, 0.000000000000000000 ) ) ;
#7244 = DIRECTION ( 'NONE',  ( -0.000000000000000000, -1.000000000000000000, -0.000000000000000000 ) ) ;
#7245 = CARTESIAN_POINT ( 'NONE',  ( -80.73480563767387252, 139.7732851794904434, 489.5387775887227235 ) ) ;
#7246 = CARTESIAN_POINT ( 'NONE',  ( -31.00000000000003553, 19.00000000000000000, 25.99999999999999645 ) ) ;
#7247 = EDGE_CURVE ( 'NONE', #10962, #6521, #1633, .T. ) ;
#7248 = ORIENTED_EDGE ( 'NONE', *, *, #13696, .F. ) ;
#7249 = PLANE ( 'NONE',  #6240 ) ;
#7250 = FACE_BOUND ( 'NONE', #16356, .T. ) ;
#7251 = ADVANCED_FACE ( 'NONE', ( #1086 ), #15907, .F. ) ;
#7252 = AXIS2_PLACEMENT_3D ( 'NONE', #5934, #19933, #7391 ) ;
#7253 =( GEOMETRIC_REPRESENTATION_CONTEXT ( 3 ) GLOBAL_UNCERTAINTY_ASSIGNED_CONTEXT ( ( #5453 ) ) GLOBAL_UNIT_ASSIGNED_CONTEXT ( ( #20315, #9591, #15911 ) ) REPRESENTATION_CONTEXT ( 'NONE', 'WORKASPACE' ) );
#7254 = VERTEX_POINT ( 'NONE', #12916 ) ;
#7255 = EDGE_CURVE ( 'NONE', #12831, #889, #3533, .T. ) ;
#7256 = ORIENTED_EDGE ( 'NONE', *, *, #20216, .F. ) ;
#7257 = DIRECTION ( 'NONE',  ( 0.000000000000000000, 0.000000000000000000, -1.000000000000000000 ) ) ;
#7258 = DIRECTION ( 'NONE',  ( -0.000000000000000000, -1.000000000000000000, -0.000000000000000000 ) ) ;
#7259 = UNCERTAINTY_MEASURE_WITH_UNIT (LENGTH_MEASURE( 1.000000000000000082E-05 ), #6985, 'distance_accuracy_value', 'NONE');
#7260 = ORIENTED_EDGE ( 'NONE', *, *, #12733, .F. ) ;
#7261 = DIRECTION ( 'NONE',  ( -0.000000000000000000, -1.000000000000000000, -0.000000000000000000 ) ) ;
#7262 =( LENGTH_UNIT ( ) NAMED_UNIT ( * ) SI_UNIT ( .MILLI., .METRE. ) );
#7264 = EDGE_CURVE ( 'NONE', #15515, #13110, #421, .T. ) ;
#7263 = SURFACE_STYLE_FILL_AREA ( #2706 ) ;
#7265 = CIRCLE ( 'NONE', #15820, 10.00000000000000888 ) ;
#7266 = DIRECTION ( 'NONE',  ( -0.7327934916262990317, -0.6804510993672779895, -8.333122608164345406E-17 ) ) ;
#7267 = AXIS2_PLACEMENT_3D ( 'NONE', #5772, #8458, #2459 ) ;
#7268 = CARTESIAN_POINT ( 'NONE',  ( -1.000000000000000888, 216.7545334744432921, 509.3921618609452935 ) ) ;
#7269 = CONICAL_SURFACE ( 'NONE', #20066, 12.97499999999999964, 0.5543074962015517304 ) ;
#7270 = MECHANICAL_DESIGN_GEOMETRIC_PRESENTATION_REPRESENTATION (  '', ( #4631 ), #9898 ) ;
#7271 = LINE ( 'NONE', #14884, #5768 ) ;
#7272 = ORIENTED_EDGE ( 'NONE', *, *, #10634, .F. ) ;
#7273 = SURFACE_SIDE_STYLE ('',( #2714 ) ) ;
#7274 = FACE_OUTER_BOUND ( 'NONE', #7182, .T. ) ;
#7275 = CARTESIAN_POINT ( 'NONE',  ( 468.8334540492694487, 134.2156642432025251, 245.0000000000000000 ) ) ;
#7276 = DIRECTION ( 'NONE',  ( 1.000000000000000000, 0.000000000000000000, 0.000000000000000000 ) ) ;
#7277 = ORIENTED_EDGE ( 'NONE', *, *, #6015, .T. ) ;
#7278 =( GEOMETRIC_REPRESENTATION_CONTEXT ( 3 ) GLOBAL_UNCERTAINTY_ASSIGNED_CONTEXT ( ( #423 ) ) GLOBAL_UNIT_ASSIGNED_CONTEXT ( ( #18425, #11861, #5971 ) ) REPRESENTATION_CONTEXT ( 'NONE', 'WORKASPACE' ) );
#7279 = EDGE_CURVE ( 'NONE', #6573, #19318, #1541, .T. ) ;
#7280 = ORIENTED_EDGE ( 'NONE', *, *, #14451, .T. ) ;
#7281 = ORIENTED_EDGE ( 'NONE', *, *, #15457, .F. ) ;
#7282 = ORIENTED_EDGE ( 'NONE', *, *, #16245, .T. ) ;
#7283 = EDGE_CURVE ( 'NONE', #19679, #4190, #1649, .T. ) ;
#7284 = VECTOR ( 'NONE', #9495, 1000.000000000000000 ) ;
#7285 = DIRECTION ( 'NONE',  ( 1.000000000000000000, 5.889072920838430686E-16, -0.000000000000000000 ) ) ;
#7286 = ORIENTED_EDGE ( 'NONE', *, *, #8773, .T. ) ;
#7287 = CYLINDRICAL_SURFACE ( 'NONE', #831, 12.00000000000000178 ) ;
#7288 = CARTESIAN_POINT ( 'NONE',  ( 35.00000000000000711, 19.00000000000000000, 20.99999999999999289 ) ) ;
#7289 = ORIENTED_EDGE ( 'NONE', *, *, #13736, .T. ) ;
#7290 = CARTESIAN_POINT ( 'NONE',  ( 0.000000000000000000, 341.0487089519837696, -115.0000000000032969 ) ) ;
#7291 = DIRECTION ( 'NONE',  ( 0.000000000000000000, 0.000000000000000000, 1.000000000000000000 ) ) ;
#7292 = CARTESIAN_POINT ( 'NONE',  ( -44.50085094405410757, 209.4098724938429541, 505.3921618609452935 ) ) ;
#7293 = FACE_OUTER_BOUND ( 'NONE', #9321, .T. ) ;
#7294 = DIRECTION ( 'NONE',  ( -0.000000000000000000, 0.7071067811865504593, -0.7071067811865445751 ) ) ;
#7295 =( LENGTH_UNIT ( ) NAMED_UNIT ( * ) SI_UNIT ( .MILLI., .METRE. ) );
#7296 = PRESENTATION_LAYER_ASSIGNMENT (  '', '', ( #8281 ) ) ;
#7297 = DIRECTION ( 'NONE',  ( -1.000000000000000000, -0.000000000000000000, 3.854941057726258312E-16 ) ) ;
#7298 = DIRECTION ( 'NONE',  ( 0.000000000000000000, 0.000000000000000000, 1.000000000000000000 ) ) ;
#7299 = VECTOR ( 'NONE', #2882, 1000.000000000000000 ) ;
#7300 = SURFACE_STYLE_USAGE ( .BOTH. , #7107 ) ;
#7301 = EDGE_LOOP ( 'NONE', ( #8124, #4775, #2899, #10115, #18594, #5625 ) ) ;
#7302 =( LENGTH_UNIT ( ) NAMED_UNIT ( * ) SI_UNIT ( .MILLI., .METRE. ) );
#7303 = ORIENTED_EDGE ( 'NONE', *, *, #3084, .F. ) ;
#7304 = ORIENTED_EDGE ( 'NONE', *, *, #15590, .T. ) ;
#7305 = CARTESIAN_POINT ( 'NONE',  ( -21.85283368562565443, 319.7545334744432353, 485.1700099148404774 ) ) ;
#7306 = VECTOR ( 'NONE', #19236, 1000.000000000000000 ) ;
#7307 = DIRECTION ( 'NONE',  ( 1.000000000000000000, 0.000000000000000000, 0.000000000000000000 ) ) ;
#7308 = DIRECTION ( 'NONE',  ( -1.000000000000000000, 0.000000000000000000, 0.000000000000000000 ) ) ;
#7309 = CARTESIAN_POINT ( 'NONE',  ( -26.00000000000002132, 10.00000000000000000, -31.00000000000003553 ) ) ;
#7310 = MECHANICAL_DESIGN_GEOMETRIC_PRESENTATION_REPRESENTATION (  '', ( #5656 ), #8605 ) ;
#7311 = CARTESIAN_POINT ( 'NONE',  ( -81.18192946987610981, 139.7545334744432637, -2.701928103162370948E-12 ) ) ;
#7312 = LINE ( 'NONE', #15455, #17649 ) ;
#7313 = SURFACE_STYLE_USAGE ( .BOTH. , #18420 ) ;
#7314 = PLANE ( 'NONE',  #6839 ) ;
#7315 = FACE_BOUND ( 'NONE', #8801, .T. ) ;
#7316 = CARTESIAN_POINT ( 'NONE',  ( 53.48937290013659407, 145.9162550801369491, 250.0000000000000000 ) ) ;
#7317 =( NAMED_UNIT ( * ) SI_UNIT ( $, .STERADIAN. ) SOLID_ANGLE_UNIT ( ) );
#7318 = AXIS2_PLACEMENT_3D ( 'NONE', #17143, #15827, #1661 ) ;
#7319 = EDGE_CURVE ( 'NONE', #21, #5614, #3217, .T. ) ;
#7320 = COLOUR_RGB ( '', 0.72549020, 0.75294118, 0.79215686) ;
#7321 = ORIENTED_EDGE ( 'NONE', *, *, #7339, .F. ) ;
#7322 = VERTEX_POINT ( 'NONE', #17525 ) ;
#7323 =( GEOMETRIC_REPRESENTATION_CONTEXT ( 3 ) GLOBAL_UNCERTAINTY_ASSIGNED_CONTEXT ( ( #13403 ) ) GLOBAL_UNIT_ASSIGNED_CONTEXT ( ( #4395, #13684, #15224 ) ) REPRESENTATION_CONTEXT ( 'NONE', 'WORKASPACE' ) );
#7324 = VECTOR ( 'NONE', #5635, 1000.000000000000000 ) ;
#7325 = DIRECTION ( 'NONE',  ( 0.000000000000000000, 0.000000000000000000, -1.000000000000000000 ) ) ;
#7326 = ORIENTED_EDGE ( 'NONE', *, *, #5276, .T. ) ;
#7327 = ORIENTED_EDGE ( 'NONE', *, *, #17792, .F. ) ;
#7328 = CARTESIAN_POINT ( 'NONE',  ( 78.48937290013660117, 145.9162550801369491, 250.0000000000000000 ) ) ;
#7329 = FACE_OUTER_BOUND ( 'NONE', #911, .T. ) ;
#7330 = CARTESIAN_POINT ( 'NONE',  ( 78.48937290013660117, 113.1299228374914208, 220.6387154965113382 ) ) ;
#7331 = VECTOR ( 'NONE', #11115, 1000.000000000000000 ) ;
#7332 =( GEOMETRIC_REPRESENTATION_CONTEXT ( 3 ) GLOBAL_UNCERTAINTY_ASSIGNED_CONTEXT ( ( #13615 ) ) GLOBAL_UNIT_ASSIGNED_CONTEXT ( ( #2939, #3040, #9336 ) ) REPRESENTATION_CONTEXT ( 'NONE', 'WORKASPACE' ) );
#7333 = FACE_OUTER_BOUND ( 'NONE', #15392, .T. ) ;
#7334 = ADVANCED_FACE ( 'NONE', ( #9708 ), #19178, .T. ) ;
#7335 = LINE ( 'NONE', #18445, #11021 ) ;
#7336 = DIRECTION ( 'NONE',  ( 0.000000000000000000, 0.000000000000000000, 1.000000000000000000 ) ) ;
#7337 = VECTOR ( 'NONE', #15842, 1000.000000000000114 ) ;
#7338 = LINE ( 'NONE', #5801, #17203 ) ;
#7339 = EDGE_CURVE ( 'NONE', #11321, #11823, #987, .T. ) ;
#7340 = LINE ( 'NONE', #14977, #10998 ) ;
#7341 = DIRECTION ( 'NONE',  ( 1.000000000000000000, 5.889072920838430686E-16, -0.000000000000000000 ) ) ;
#7342 = CARTESIAN_POINT ( 'NONE',  ( -79.98710143421158136, 138.7963597474245603, 490.1983628228959446 ) ) ;
#7343 = EDGE_LOOP ( 'NONE', ( #18648, #16864, #850, #908 ) ) ;
#7344 = CARTESIAN_POINT ( 'NONE',  ( 30.99999999999999645, 3.000000000000000000, 26.00000000000000355 ) ) ;
#7345 = AXIS2_PLACEMENT_3D ( 'NONE', #18755, #2684, #14119 ) ;
#7346 = ORIENTED_EDGE ( 'NONE', *, *, #2069, .F. ) ;
#7347 = DIRECTION ( 'NONE',  ( 1.000000000000000000, 0.000000000000000000, 0.000000000000000000 ) ) ;
#7348 = FACE_BOUND ( 'NONE', #10158, .T. ) ;
#7349 = AXIS2_PLACEMENT_3D ( 'NONE', #11566, #11465, #12924 ) ;
#7350 = COLOUR_RGB ( '', 0.72549020, 0.75294118, 0.79215686) ;
#7351 = EDGE_CURVE ( 'NONE', #7872, #20367, #7952, .T. ) ;
#7352 = EDGE_LOOP ( 'NONE', ( #6783, #18586 ) ) ;
#7353 = EDGE_CURVE ( 'NONE', #12074, #1376, #6629, .T. ) ;
#7354 = ORIENTED_EDGE ( 'NONE', *, *, #9483, .F. ) ;
#7355 = CARTESIAN_POINT ( 'NONE',  ( 0.000000000000000000, 0.000000000000000000, 250.0000000000000000 ) ) ;
#7356 = CARTESIAN_POINT ( 'NONE',  ( 153.4893729001366864, 103.1299228374914492, 29.36128450348865471 ) ) ;
#7357 = EDGE_LOOP ( 'NONE', ( #13022, #8293, #14870, #3142 ) ) ;
#7358 = LINE ( 'NONE', #649, #7890 ) ;
#7359 = CARTESIAN_POINT ( 'NONE',  ( 0.000000000000000000, 0.000000000000000000, 0.000000000000000000 ) ) ;
#7360 = CARTESIAN_POINT ( 'NONE',  ( 40.00000000000000711, 19.00000000000000000, 25.99999999999999645 ) ) ;
#7361 = VECTOR ( 'NONE', #1624, 1000.000000000000000 ) ;
#7362 = ADVANCED_FACE ( 'NONE', ( #116 ), #17425, .F. ) ;
#7363 = DIRECTION ( 'NONE',  ( 0.000000000000000000, 0.000000000000000000, 1.000000000000000000 ) ) ;
#7364 = DIRECTION ( 'NONE',  ( -0.000000000000000000, -1.000000000000000000, -0.000000000000000000 ) ) ;
#7365 = ORIENTED_EDGE ( 'NONE', *, *, #2722, .F. ) ;
#7366 = DIRECTION ( 'NONE',  ( 0.000000000000000000, 0.000000000000000000, -1.000000000000000000 ) ) ;
#7367 = ADVANCED_FACE ( 'NONE', ( #18862 ), #6317, .F. ) ;
#7368 =( REPRESENTATION_RELATIONSHIP ('NONE','NONE', #12483, #10923 ) REPRESENTATION_RELATIONSHIP_WITH_TRANSFORMATION ( #14365 )SHAPE_REPRESENTATION_RELATIONSHIP( ) );
#7369 = CARTESIAN_POINT ( 'NONE',  ( -1.000000000000013545, 138.3494706343262237, 489.1604469778678776 ) ) ;
#7370 = DIRECTION ( 'NONE',  ( 0.000000000000000000, 1.000000000000000000, 0.000000000000000000 ) ) ;
#7371 = CARTESIAN_POINT ( 'NONE',  ( 55.06686112950496437, 310.4499764460939559, 214.9384415106391373 ) ) ;
#7372 = MECHANICAL_DESIGN_GEOMETRIC_PRESENTATION_REPRESENTATION (  '', ( #6085 ), #9331 ) ;
#7373 = VERTEX_POINT ( 'NONE', #16332 ) ;
#7374 = ORIENTED_EDGE ( 'NONE', *, *, #5488, .T. ) ;
#7375 = CARTESIAN_POINT ( 'NONE',  ( 39.99999999999999289, 0.000000000000000000, 26.00000000000000000 ) ) ;
#7376 = ORIENTED_EDGE ( 'NONE', *, *, #15699, .F. ) ;
#7377 = AXIS2_PLACEMENT_3D ( 'NONE', #6452, #4686, #18898 ) ;
#7378 = ORIENTED_EDGE ( 'NONE', *, *, #16628, .F. ) ;
#7379 = EDGE_CURVE ( 'NONE', #10589, #20130, #17835, .T. ) ;
#7380 = ORIENTED_EDGE ( 'NONE', *, *, #8140, .F. ) ;
#7381 =( GEOMETRIC_REPRESENTATION_CONTEXT ( 3 ) GLOBAL_UNCERTAINTY_ASSIGNED_CONTEXT ( ( #11773 ) ) GLOBAL_UNIT_ASSIGNED_CONTEXT ( ( #17007, #12461, #7613 ) ) REPRESENTATION_CONTEXT ( 'NONE', 'WORKASPACE' ) );
#7382 = VECTOR ( 'NONE', #8798, 1000.000000000000000 ) ;
#7383 = AXIS2_PLACEMENT_3D ( 'NONE', #14667, #632, #14551 ) ;
#7384 = CARTESIAN_POINT ( 'NONE',  ( 40.00000000000000711, 11.00000000000000000, 34.99999999999997868 ) ) ;
#7385 = ORIENTED_EDGE ( 'NONE', *, *, #13467, .F. ) ;
#7386 = DIRECTION ( 'NONE',  ( -0.000000000000000000, 0.7817866094812239153, 0.6235460666509350380 ) ) ;
#7387 = ORIENTED_EDGE ( 'NONE', *, *, #18049, .T. ) ;
#7388 = EDGE_CURVE ( 'NONE', #16045, #12183, #3734, .T. ) ;
#7389 = CARTESIAN_POINT ( 'NONE',  ( -3.000000000000000000, -1.836909530733565148E-16, 3.000000000000000000 ) ) ;
#7390 = PRESENTATION_LAYER_ASSIGNMENT (  '', '', ( #4095 ) ) ;
#7391 = DIRECTION ( 'NONE',  ( 0.000000000000000000, 0.9980168174369414835, 0.06294785233063035501 ) ) ;
#7392 = EDGE_CURVE ( 'NONE', #19303, #15899, #11889, .T. ) ;
#7393 = LINE ( 'NONE', #17158, #19384 ) ;
#7394 = CARTESIAN_POINT ( 'NONE',  ( 10.00000000000000000, 309.2289037985885898, -83.18019484660915452 ) ) ;
#7395 = CARTESIAN_POINT ( 'NONE',  ( 10.00000000000000000, 372.8685141053783241, -150.1198051533980049 ) ) ;
#7396 = CIRCLE ( 'NONE', #17580, 12.00000000000000178 ) ;
#7397 = AXIS2_PLACEMENT_3D ( 'NONE', #16507, #5474, #7134 ) ;
#7398 = CARTESIAN_POINT ( 'NONE',  ( -34.99999999999998579, 0.000000000000000000, 18.50000000000000355 ) ) ;
#7399 = CARTESIAN_POINT ( 'NONE',  ( -41.50085094405408626, 209.4098724938429541, 505.3921618609452935 ) ) ;
#7401 = STYLED_ITEM ( 'NONE', ( #6415 ), #15054 ) ;
#7400 = FACE_OUTER_BOUND ( 'NONE', #16564, .T. ) ;
#7402 = PRESENTATION_STYLE_ASSIGNMENT (( #12047 ) ) ;
#7403 = STYLED_ITEM ( 'NONE', ( #818 ), #16014 ) ;
#7404 = CARTESIAN_POINT ( 'NONE',  ( -37.00000000000000000, 0.000000000000000000, 23.00000000000000355 ) ) ;
#7405 = CARTESIAN_POINT ( 'NONE',  ( -58.16843972078500258, 319.7545334744432353, 489.0536462814662286 ) ) ;
#7406 = CARTESIAN_POINT ( 'NONE',  ( 39.99999999999999289, 8.000000000000000000, 18.99999999999999645 ) ) ;
#7407 = EDGE_LOOP ( 'NONE', ( #6492, #14730, #19998, #10254, #18668, #6399 ) ) ;
#7408 = COLOUR_RGB ( '', 0.09019608, 0.27058824, 0.51372549) ;
#7409 = COLOUR_RGB ( '', 0.66274510, 0.83137255, 0.94901961) ;
#7410 = EDGE_LOOP ( 'NONE', ( #7533, #6329, #3082, #5033 ) ) ;
#7411 = PRODUCT_DEFINITION_CONTEXT ( 'detailed design', #4217, 'design' ) ;
#7412 = MECHANICAL_DESIGN_GEOMETRIC_PRESENTATION_REPRESENTATION (  '', ( #12035 ), #16316 ) ;
#7413 = ORIENTED_EDGE ( 'NONE', *, *, #5148, .F. ) ;
#7415 = ORIENTED_EDGE ( 'NONE', *, *, #1812, .F. ) ;
#7414 = EDGE_CURVE ( 'NONE', #10365, #19318, #5487, .T. ) ;
#7416 = VECTOR ( 'NONE', #3543, 1000.000000000000000 ) ;
#7417 = CARTESIAN_POINT ( 'NONE',  ( -78.99999999999995737, 138.7545334744432637, 477.3411705753777596 ) ) ;
#7418 = ORIENTED_EDGE ( 'NONE', *, *, #15149, .F. ) ;
#7419 = LINE ( 'NONE', #13497, #458 ) ;
#7420 = LINE ( 'NONE', #17362, #14490 ) ;
#7421 = AXIS2_PLACEMENT_3D ( 'NONE', #3962, #16545, #3567 ) ;
#7422 = FACE_OUTER_BOUND ( 'NONE', #391, .T. ) ;
#7423 = EDGE_CURVE ( 'NONE', #6147, #825, #17133, .T. ) ;
#7424 =( LENGTH_UNIT ( ) NAMED_UNIT ( * ) SI_UNIT ( .MILLI., .METRE. ) );
#7425 = DIRECTION ( 'NONE',  ( -0.000000000000000000, 1.000000000000000000, -0.000000000000000000 ) ) ;
#7426 = CARTESIAN_POINT ( 'NONE',  ( -32.00000000000000711, 6.000000000000000000, -23.00000000000000000 ) ) ;
#7427 = CARTESIAN_POINT ( 'NONE',  ( 0.000000000000000000, 309.2289037985885898, -79.88019484660914316 ) ) ;
#7428 = CARTESIAN_POINT ( 'NONE',  ( 5.687501635565830327, -12.64907335584850046, 1.549064719741993485E-15 ) ) ;
#7429 = PRESENTATION_LAYER_ASSIGNMENT (  '', '', ( #6085 ) ) ;
#7430 = SURFACE_STYLE_USAGE ( .BOTH. , #9067 ) ;
#7431 = VECTOR ( 'NONE', #7285, 1000.000000000000000 ) ;
#7432 = CARTESIAN_POINT ( 'NONE',  ( -22.00000000000001776, 10.00000000000000000, 32.00000000000000711 ) ) ;
#7433 = DIRECTION ( 'NONE',  ( 1.000000000000000000, -0.000000000000000000, -0.000000000000000000 ) ) ;
#7434 = CYLINDRICAL_SURFACE ( 'NONE', #15165, 10.00000000000000888 ) ;
#7435 = CARTESIAN_POINT ( 'NONE',  ( 21.00000000000000000, 19.00000000000000000, 35.00000000000001421 ) ) ;
#7436 = VECTOR ( 'NONE', #13135, 1000.000000000000000 ) ;
#7437 = VERTEX_POINT ( 'NONE', #4031 ) ;
#7438 = ORIENTED_EDGE ( 'NONE', *, *, #15437, .T. ) ;
#7439 = AXIS2_PLACEMENT_3D ( 'NONE', #8575, #17963, #3945 ) ;
#7440 = ADVANCED_FACE ( 'NONE', ( #620 ), #9912, .F. ) ;
#7441 = ORIENTED_EDGE ( 'NONE', *, *, #1780, .T. ) ;
#7442 = EDGE_LOOP ( 'NONE', ( #9884, #6098, #19348, #12598 ) ) ;
#7443 = DIRECTION ( 'NONE',  ( 1.000000000000000000, 0.000000000000000000, 0.000000000000000000 ) ) ;
#7444 = MECHANICAL_DESIGN_GEOMETRIC_PRESENTATION_REPRESENTATION (  '', ( #16015 ), #2484 ) ;
#7445 = DIRECTION ( 'NONE',  ( 1.000000000000000000, 0.000000000000000000, 0.000000000000000000 ) ) ;
#7446 = UNCERTAINTY_MEASURE_WITH_UNIT (LENGTH_MEASURE( 1.000000000000000082E-05 ), #19994, 'distance_accuracy_value', 'NONE');
#7447 = CARTESIAN_POINT ( 'NONE',  ( -1.000000000000008216, 144.4616402556298453, 504.6850550797586834 ) ) ;
#7448 = CARTESIAN_POINT ( 'NONE',  ( -37.00000000000000711, 6.000000000000000000, -23.00000000000000000 ) ) ;
#7449 = FACE_OUTER_BOUND ( 'NONE', #12090, .T. ) ;
#7450 =( LENGTH_UNIT ( ) NAMED_UNIT ( * ) SI_UNIT ( .MILLI., .METRE. ) );
#7451 = EDGE_CURVE ( 'NONE', #20355, #3507, #11458, .T. ) ;
#7452 = CARTESIAN_POINT ( 'NONE',  ( 10.00000000000000000, 381.0487089519832011, -80.00000000000332534 ) ) ;
#7453 = CARTESIAN_POINT ( 'NONE',  ( 98.48937290013662960, 1.571051285554951424E-14, 250.0000000000000000 ) ) ;
#7454 = CARTESIAN_POINT ( 'NONE',  ( 39.99999999999999289, 10.00000000000000000, -26.00000000000000000 ) ) ;
#7455 = DIRECTION ( 'NONE',  ( 0.000000000000000000, 0.000000000000000000, -1.000000000000000000 ) ) ;
#7456 = AXIS2_PLACEMENT_3D ( 'NONE', #5171, #11444, #1735 ) ;
#7457 = CARTESIAN_POINT ( 'NONE',  ( -80.12162488254176651, 138.9594563584317086, 489.0814894912512045 ) ) ;
#7458 = DIRECTION ( 'NONE',  ( 1.000000000000000000, -0.000000000000000000, 0.000000000000000000 ) ) ;
#7459 = ORIENTED_EDGE ( 'NONE', *, *, #3120, .T. ) ;
#7460 = DIRECTION ( 'NONE',  ( 3.854941057726247958E-16, -0.000000000000000000, 1.000000000000000000 ) ) ;
#7461 = CARTESIAN_POINT ( 'NONE',  ( -39.99999999999997868, 3.000000000000000000, 26.00000000000000355 ) ) ;
#7462 =( NAMED_UNIT ( * ) SI_UNIT ( $, .STERADIAN. ) SOLID_ANGLE_UNIT ( ) );
#7463 = AXIS2_PLACEMENT_3D ( 'NONE', #15156, #5307, #1000 ) ;
#7464 = ORIENTED_EDGE ( 'NONE', *, *, #6142, .T. ) ;
#7465 = EDGE_CURVE ( 'NONE', #9346, #12110, #15178, .T. ) ;
#7466 = UNCERTAINTY_MEASURE_WITH_UNIT (LENGTH_MEASURE( 1.000000000000000082E-05 ), #12633, 'distance_accuracy_value', 'NONE');
#7467 = ORIENTED_EDGE ( 'NONE', *, *, #2971, .F. ) ;
#7468 = CARTESIAN_POINT ( 'NONE',  ( 31.81980515339464333, 0.000000000000000000, 28.51980515339463906 ) ) ;
#7469 = CARTESIAN_POINT ( 'NONE',  ( 7.000000000000000000, 0.000000000000000000, 0.000000000000000000 ) ) ;
#7470 = TOROIDAL_SURFACE ( 'NONE', #9761, 8.000000000000000000, 1.000000000000000000 ) ;
#7471 = EDGE_LOOP ( 'NONE', ( #1149, #14629, #5507, #8819 ) ) ;
#7472 = CARTESIAN_POINT ( 'NONE',  ( 0.000000000000000000, 372.8685141053783241, -143.5198051533979537 ) ) ;
#7473 = CARTESIAN_POINT ( 'NONE',  ( 25.99999999999999645, 0.000000000000000000, 31.00000000000004619 ) ) ;
#7474 =( NAMED_UNIT ( * ) PLANE_ANGLE_UNIT ( ) SI_UNIT ( $, .RADIAN. ) );
#7475 = EDGE_CURVE ( 'NONE', #17493, #19448, #6939, .T. ) ;
#7476 = DIRECTION ( 'NONE',  ( 1.000000000000000000, 0.000000000000000000, -0.000000000000000000 ) ) ;
#7477 = VERTEX_POINT ( 'NONE', #10210 ) ;
#7478 = CARTESIAN_POINT ( 'NONE',  ( 22.99999999999999289, 0.000000000000000000, 37.00000000000002132 ) ) ;
#7479 = CARTESIAN_POINT ( 'NONE',  ( 53.48937290013659407, 145.9162550801369491, 250.0000000000000000 ) ) ;
#7480 = DIRECTION ( 'NONE',  ( 1.000000000000000000, 0.000000000000000000, 0.000000000000000000 ) ) ;
#7481 = ORIENTED_EDGE ( 'NONE', *, *, #4294, .T. ) ;
#7482 = EDGE_LOOP ( 'NONE', ( #15356, #38 ) ) ;
#7483 = PRODUCT_RELATED_PRODUCT_CATEGORY ( 'part', '', ( #16206 ) ) ;
#7484 = SURFACE_SIDE_STYLE ('',( #11811 ) ) ;
#7485 = VERTEX_POINT ( 'NONE', #11874 ) ;
#7486 = VERTEX_POINT ( 'NONE', #5384 ) ;
#7487 = ORIENTED_EDGE ( 'NONE', *, *, #14155, .F. ) ;
#7488 = CARTESIAN_POINT ( 'NONE',  ( 35.00000000000003553, -20.00000000000000000, -18.49999999999999645 ) ) ;
#7489 = ORIENTED_EDGE ( 'NONE', *, *, #15818, .F. ) ;
#7490 = EDGE_CURVE ( 'NONE', #889, #2901, #10319, .T. ) ;
#7491 = CARTESIAN_POINT ( 'NONE',  ( -20.99999999999999645, 8.000000000000000000, 35.00000000000001421 ) ) ;
#7492 = VERTEX_POINT ( 'NONE', #19580 ) ;
#7493 = VECTOR ( 'NONE', #16612, 1000.000000000000000 ) ;
#7494 = DIRECTION ( 'NONE',  ( -1.000000000000000000, 0.000000000000000000, 0.000000000000000000 ) ) ;
#7495 = DIRECTION ( 'NONE',  ( 1.000000000000000000, 0.000000000000000000, 0.000000000000000000 ) ) ;
#7496 =( NAMED_UNIT ( * ) PLANE_ANGLE_UNIT ( ) SI_UNIT ( $, .RADIAN. ) );
#7497 = ADVANCED_FACE ( 'NONE', ( #8373, #5187 ), #14655, .T. ) ;
#7498 = CARTESIAN_POINT ( 'NONE',  ( -20.99999999999999645, 19.00000000000000000, -35.00000000000000711 ) ) ;
#7499 = DIRECTION ( 'NONE',  ( 0.000000000000000000, -1.000000000000000000, 0.000000000000000000 ) ) ;
#7500 = DIRECTION ( 'NONE',  ( 0.000000000000000000, 0.000000000000000000, -1.000000000000000000 ) ) ;
#7501 = ADVANCED_FACE ( 'NONE', ( #14967 ), #13330, .F. ) ;
#7502 = DIRECTION ( 'NONE',  ( 0.000000000000000000, 1.000000000000000000, 0.000000000000000000 ) ) ;
#7503 = LINE ( 'NONE', #15343, #13491 ) ;
#7504 = VECTOR ( 'NONE', #16757, 1000.000000000000000 ) ;
#7505 = ORIENTED_EDGE ( 'NONE', *, *, #13557, .F. ) ;
#7506 = EDGE_CURVE ( 'NONE', #1681, #4967, #18344, .T. ) ;
#7507 = CIRCLE ( 'NONE', #4214, 4.999999999999990230 ) ;
#7508 = ORIENTED_EDGE ( 'NONE', *, *, #2046, .F. ) ;
#7509 = ADVANCED_FACE ( 'NONE', ( #15480 ), #2783, .T. ) ;
#7510 = ORIENTED_EDGE ( 'NONE', *, *, #19672, .F. ) ;
#7511 = ORIENTED_EDGE ( 'NONE', *, *, #10523, .T. ) ;
#7512 =( NAMED_UNIT ( * ) PLANE_ANGLE_UNIT ( ) SI_UNIT ( $, .RADIAN. ) );
#7513 = VERTEX_POINT ( 'NONE', #7234 ) ;
#7514 = DIRECTION ( 'NONE',  ( 1.000000000000000000, -0.000000000000000000, 0.000000000000000000 ) ) ;
#7515 = CARTESIAN_POINT ( 'NONE',  ( -21.85283368562565443, 319.7545334744432353, 485.1700099148404774 ) ) ;
#7516 = ORIENTED_EDGE ( 'NONE', *, *, #15828, .T. ) ;
#7517 = DIRECTION ( 'NONE',  ( -1.000000000000000000, 0.000000000000000000, -0.000000000000000000 ) ) ;
#7518 = CARTESIAN_POINT ( 'NONE',  ( 503.8334540492693918, 191.8198460455371333, 81.76606011801540319 ) ) ;
#7519 = CARTESIAN_POINT ( 'NONE',  ( -23.00000000000003197, 3.000000000000000000, 34.00000000000000711 ) ) ;
#7520 = AXIS2_PLACEMENT_3D ( 'NONE', #19111, #17274, #9752 ) ;
#7521 = DIRECTION ( 'NONE',  ( 1.000000000000000000, 0.000000000000000000, 0.000000000000000000 ) ) ;
#7522 =( NAMED_UNIT ( * ) SI_UNIT ( $, .STERADIAN. ) SOLID_ANGLE_UNIT ( ) );
#7523 = DIRECTION ( 'NONE',  ( 1.000000000000000000, 0.000000000000000000, 0.000000000000000000 ) ) ;
#7524 = PLANE ( 'NONE',  #994 ) ;
#7525 = DIRECTION ( 'NONE',  ( 0.000000000000000000, 0.000000000000000000, 1.000000000000000000 ) ) ;
#7526 = ADVANCED_FACE ( 'NONE', ( #9172 ), #17023, .T. ) ;
#7527 = ORIENTED_EDGE ( 'NONE', *, *, #17356, .F. ) ;
#7528 = ORIENTED_EDGE ( 'NONE', *, *, #12663, .T. ) ;
#7529 = EDGE_LOOP ( 'NONE', ( #7115, #17553, #12867, #18600 ) ) ;
#7531 = ADVANCED_FACE ( 'NONE', ( #12167 ), #10824, .T. ) ;
#7530 = AXIS2_PLACEMENT_3D ( 'NONE', #7667, #18779, #3231 ) ;
#7532 = EDGE_LOOP ( 'NONE', ( #17519, #17834, #8800, #19546 ) ) ;
#7533 = ORIENTED_EDGE ( 'NONE', *, *, #18671, .T. ) ;
#7534 = CARTESIAN_POINT ( 'NONE',  ( 111.4893729001366012, 127.7247684487574304, 252.0000000000000000 ) ) ;
#7535 = EDGE_CURVE ( 'NONE', #16867, #10095, #4545, .T. ) ;
#7536 = ORIENTED_EDGE ( 'NONE', *, *, #17686, .F. ) ;
#7537 = SURFACE_STYLE_USAGE ( .BOTH. , #2577 ) ;
#7538 = CARTESIAN_POINT ( 'NONE',  ( -82.18192946989263703, 139.7545334744432637, 496.6642397995873921 ) ) ;
#7539 = SURFACE_SIDE_STYLE ('',( #19883 ) ) ;
#7540 = SURFACE_SIDE_STYLE ('',( #15378 ) ) ;
#7541 = DIRECTION ( 'NONE',  ( 0.000000000000000000, 1.000000000000000000, 0.000000000000000000 ) ) ;
#7542 = LINE ( 'NONE', #5991, #19481 ) ;
#7543 = CARTESIAN_POINT ( 'NONE',  ( 0.000000000000000000, 0.000000000000000000, -34.00000000000000000 ) ) ;
#7544 = CARTESIAN_POINT ( 'NONE',  ( 78.48937290013660117, 113.1299228374914208, 79.58252780074349175 ) ) ;
#7545 = VECTOR ( 'NONE', #19263, 1000.000000000000000 ) ;
#7546 = VERTEX_POINT ( 'NONE', #17104 ) ;
#7547 = VECTOR ( 'NONE', #19610, 1000.000000000000000 ) ;
#7548 = DIRECTION ( 'NONE',  ( 0.000000000000000000, 1.000000000000000000, 0.000000000000000000 ) ) ;
#7549 = ADVANCED_FACE ( 'NONE', ( #10618 ), #4245, .T. ) ;
#7550 = EDGE_LOOP ( 'NONE', ( #18651, #6401, #13461, #9150 ) ) ;
#7551 = MECHANICAL_DESIGN_GEOMETRIC_PRESENTATION_REPRESENTATION (  '', ( #13842 ), #3619 ) ;
#7552 = PRESENTATION_LAYER_ASSIGNMENT (  '', '', ( #12833 ) ) ;
#7553 = VECTOR ( 'NONE', #19402, 1000.000000000000000 ) ;
#7554 = ORIENTED_EDGE ( 'NONE', *, *, #527, .T. ) ;
#7555 = DIRECTION ( 'NONE',  ( -0.000000000000000000, -1.000000000000000000, -0.000000000000000000 ) ) ;
#7556 = DIRECTION ( 'NONE',  ( 0.000000000000000000, 1.000000000000000000, 0.000000000000000000 ) ) ;
#7557 = ORIENTED_EDGE ( 'NONE', *, *, #3952, .F. ) ;
#7558 = CARTESIAN_POINT ( 'NONE',  ( -21.00000000000002842, 3.000000000000000000, -32.49999999999999289 ) ) ;
#7559 = SURFACE_SIDE_STYLE ('',( #1228 ) ) ;
#7560 = DIRECTION ( 'NONE',  ( -8.673617379884027583E-16, 0.000000000000000000, 1.000000000000000000 ) ) ;
#7561 = CARTESIAN_POINT ( 'NONE',  ( -78.99999999999995737, 216.7545334744432921, 478.3411705753777596 ) ) ;
#7562 = CARTESIAN_POINT ( 'NONE',  ( -30.99999999999999645, 68.00000000000000000, -30.99999999999999289 ) ) ;
#7563 = DIRECTION ( 'NONE',  ( 1.000000000000000000, 0.000000000000000000, -7.709882115452498874E-16 ) ) ;
#7564 = ORIENTED_EDGE ( 'NONE', *, *, #19057, .T. ) ;
#7565 = DIRECTION ( 'NONE',  ( 0.000000000000000000, -0.000000000000000000, -1.000000000000000000 ) ) ;
#7566 = ORIENTED_EDGE ( 'NONE', *, *, #11893, .T. ) ;
#7567 = CARTESIAN_POINT ( 'NONE',  ( -35.00000000000000000, 19.00000000000000000, -21.00000000000000000 ) ) ;
#7568 = FILL_AREA_STYLE ('',( #1236 ) ) ;
#7569 = APPLICATION_PROTOCOL_DEFINITION ( 'draft international standard', 'automotive_design', 1998, #8957 ) ;
#7570 =( GEOMETRIC_REPRESENTATION_CONTEXT ( 3 ) GLOBAL_UNCERTAINTY_ASSIGNED_CONTEXT ( ( #19636 ) ) GLOBAL_UNIT_ASSIGNED_CONTEXT ( ( #9297, #18768, #2900 ) ) REPRESENTATION_CONTEXT ( 'NONE', 'WORKASPACE' ) );
#7571 = EDGE_LOOP ( 'NONE', ( #4752, #9858, #13806, #3555 ) ) ;
#7572 = VERTEX_POINT ( 'NONE', #10520 ) ;
#7573 = ORIENTED_EDGE ( 'NONE', *, *, #16350, .F. ) ;
#7574 = ORIENTED_EDGE ( 'NONE', *, *, #8372, .F. ) ;
#7575 = CARTESIAN_POINT ( 'NONE',  ( 34.99999999999997868, 8.000000000000000000, 40.00000000000000711 ) ) ;
#7576 = ORIENTED_EDGE ( 'NONE', *, *, #3338, .F. ) ;
#7577 = DIRECTION ( 'NONE',  ( 0.000000000000000000, -1.000000000000000000, -7.137148015447440312E-15 ) ) ;
#7578 = COLOUR_RGB ( '', 0.66274510, 0.83137255, 0.94901961) ;
#7579 =( NAMED_UNIT ( * ) PLANE_ANGLE_UNIT ( ) SI_UNIT ( $, .RADIAN. ) );
#7580 = CONICAL_SURFACE ( 'NONE', #9560, 14.92500000000000071, 1.076854957875310381 ) ;
#7581 =( GEOMETRIC_REPRESENTATION_CONTEXT ( 3 ) GLOBAL_UNCERTAINTY_ASSIGNED_CONTEXT ( ( #18004 ) ) GLOBAL_UNIT_ASSIGNED_CONTEXT ( ( #8674, #5797, #2373 ) ) REPRESENTATION_CONTEXT ( 'NONE', 'WORKASPACE' ) );
#7582 = SURFACE_STYLE_FILL_AREA ( #4900 ) ;
#7583 = FACE_OUTER_BOUND ( 'NONE', #4678, .T. ) ;
#7584 = DIRECTION ( 'NONE',  ( 0.000000000000000000, 1.000000000000000000, 0.000000000000000000 ) ) ;
#7585 = DIRECTION ( 'NONE',  ( 1.000000000000000000, -0.000000000000000000, 3.854941057726254860E-16 ) ) ;
#7586 = DIRECTION ( 'NONE',  ( -6.123031769111888756E-17, 0.000000000000000000, -1.000000000000000000 ) ) ;
#7587 = CARTESIAN_POINT ( 'NONE',  ( 10.00000000000000000, 376.0487089519831443, -75.00000000000331113 ) ) ;
#7588 = EDGE_CURVE ( 'NONE', #11175, #3837, #16511, .T. ) ;
#7589 = DIRECTION ( 'NONE',  ( 0.000000000000000000, 0.000000000000000000, 1.000000000000000000 ) ) ;
#7590 = DIRECTION ( 'NONE',  ( 0.3832643291392058282, 0.000000000000000000, 0.9236387031786154056 ) ) ;
#7591 =( LENGTH_UNIT ( ) NAMED_UNIT ( * ) SI_UNIT ( .MILLI., .METRE. ) );
#7592 = DIRECTION ( 'NONE',  ( 0.000000000000000000, 0.000000000000000000, -1.000000000000000000 ) ) ;
#7593 = DIRECTION ( 'NONE',  ( 1.000000000000000000, 9.815121534730717399E-17, 0.000000000000000000 ) ) ;
#7594 = CARTESIAN_POINT ( 'NONE',  ( -40.00000000000000711, 6.000000000000000000, -18.00000000000000355 ) ) ;
#7595 = AXIS2_PLACEMENT_3D ( 'NONE', #12728, #11863, #6760 ) ;
#7596 = AXIS2_PLACEMENT_3D ( 'NONE', #1637, #6520, #11243 ) ;
#7597 = ORIENTED_EDGE ( 'NONE', *, *, #3587, .F. ) ;
#7598 = ORIENTED_EDGE ( 'NONE', *, *, #9777, .F. ) ;
#7599 = PRODUCT ( 'Part12^Assem2', 'Part12^Assem2', '', ( #5830 ) ) ;
#7600 = EDGE_CURVE ( 'NONE', #19512, #2627, #2985, .T. ) ;
#7601 = ORIENTED_EDGE ( 'NONE', *, *, #14957, .T. ) ;
#7602 = DIRECTION ( 'NONE',  ( 0.000000000000000000, 0.000000000000000000, -1.000000000000000000 ) ) ;
#7603 = FACE_OUTER_BOUND ( 'NONE', #771, .T. ) ;
#7604 = ORIENTED_EDGE ( 'NONE', *, *, #1817, .T. ) ;
#7605 = SHAPE_REPRESENTATION ( '722909', ( #2741 ), #4683 ) ;
#7606 = DIRECTION ( 'NONE',  ( 0.000000000000000000, 1.000000000000000000, 0.000000000000000000 ) ) ;
#7607 = EDGE_CURVE ( 'NONE', #4620, #20287, #14846, .T. ) ;
#7608 = VERTEX_POINT ( 'NONE', #19771 ) ;
#7609 =( GEOMETRIC_REPRESENTATION_CONTEXT ( 3 ) GLOBAL_UNCERTAINTY_ASSIGNED_CONTEXT ( ( #10728 ) ) GLOBAL_UNIT_ASSIGNED_CONTEXT ( ( #4843, #1401, #11023 ) ) REPRESENTATION_CONTEXT ( 'NONE', 'WORKASPACE' ) );
#7610 = DIRECTION ( 'NONE',  ( 0.000000000000000000, 0.000000000000000000, 1.000000000000000000 ) ) ;
#7611 = EDGE_CURVE ( 'NONE', #19713, #18686, #20084, .T. ) ;
#7612 = CARTESIAN_POINT ( 'NONE',  ( 133.4893729001365728, 167.9162550801369491, -97.94896630388704750 ) ) ;
#7613 =( NAMED_UNIT ( * ) SI_UNIT ( $, .STERADIAN. ) SOLID_ANGLE_UNIT ( ) );
#7614 = LINE ( 'NONE', #7432, #433 ) ;
#7615 = CARTESIAN_POINT ( 'NONE',  ( 53.48937290013660828, 34.32473510485366575, 250.0000000000000000 ) ) ;
#7616 = PLANE ( 'NONE',  #14520 ) ;
#7617 = LINE ( 'NONE', #16717, #1980 ) ;
#7618 = SURFACE_STYLE_FILL_AREA ( #1292 ) ;
#7619 = EDGE_CURVE ( 'NONE', #21, #7608, #5676, .T. ) ;
#7620 = EDGE_LOOP ( 'NONE', ( #8694, #3814, #6704, #13219 ) ) ;
#7621 = AXIS2_PLACEMENT_3D ( 'NONE', #3998, #6056, #13488 ) ;
#7622 = ORIENTED_EDGE ( 'NONE', *, *, #8145, .F. ) ;
#7623 = ORIENTED_EDGE ( 'NONE', *, *, #4793, .F. ) ;
#7624 = ORIENTED_EDGE ( 'NONE', *, *, #9503, .F. ) ;
#7625 = EDGE_CURVE ( 'NONE', #19819, #3908, #2578, .T. ) ;
#7626 = DIRECTION ( 'NONE',  ( 1.000000000000000000, -0.000000000000000000, -0.000000000000000000 ) ) ;
#7627 = VERTEX_POINT ( 'NONE', #8870 ) ;
#7628 = ORIENTED_EDGE ( 'NONE', *, *, #17686, .T. ) ;
#7629 = ORIENTED_EDGE ( 'NONE', *, *, #16565, .F. ) ;
#7630 = DIRECTION ( 'NONE',  ( -0.000000000000000000, -1.000000000000000000, -0.000000000000000000 ) ) ;
#7631 = CARTESIAN_POINT ( 'NONE',  ( -26.00000000000000000, 19.00000000000000000, -40.00000000000000711 ) ) ;
#7632 = UNCERTAINTY_MEASURE_WITH_UNIT (LENGTH_MEASURE( 1.000000000000000082E-05 ), #9447, 'distance_accuracy_value', 'NONE');
#7633 = DIRECTION ( 'NONE',  ( -1.000000000000000000, -2.135044278125301096E-16, -0.000000000000000000 ) ) ;
#7634 = DIRECTION ( 'NONE',  ( 1.000000000000000000, -0.000000000000000000, -0.000000000000000000 ) ) ;
#7635 = DIRECTION ( 'NONE',  ( 1.000000000000000000, 0.000000000000000000, 0.000000000000000000 ) ) ;
#7636 = EDGE_CURVE ( 'NONE', #8829, #10868, #1003, .T. ) ;
#7637 = PLANE ( 'NONE',  #96 ) ;
#7638 = LINE ( 'NONE', #9278, #11618 ) ;
#7639 = MECHANICAL_DESIGN_GEOMETRIC_PRESENTATION_REPRESENTATION (  '', ( #17176 ), #17839 ) ;
#7640 = EDGE_CURVE ( 'NONE', #19421, #12712, #15186, .T. ) ;
#7641 = DIRECTION ( 'NONE',  ( -0.000000000000000000, -1.000000000000000000, -0.000000000000000000 ) ) ;
#7642 = AXIS2_PLACEMENT_3D ( 'NONE', #13477, #4385, #1250 ) ;
#7643 = ORIENTED_EDGE ( 'NONE', *, *, #5848, .F. ) ;
#7644 = DIRECTION ( 'NONE',  ( -1.000000000000000000, 0.000000000000000000, 0.000000000000000000 ) ) ;
#7645 = CARTESIAN_POINT ( 'NONE',  ( 31.00000000000004263, 68.00000000000000000, -25.99999999999999645 ) ) ;
#7646 = AXIS2_PLACEMENT_3D ( 'NONE', #2103, #569, #6877 ) ;
#7647 = ORIENTED_EDGE ( 'NONE', *, *, #6105, .T. ) ;
#7648 = CIRCLE ( 'NONE', #8952, 10.00000000000000888 ) ;
#7649 = CIRCLE ( 'NONE', #14236, 2.500000000000002220 ) ;
#7650 = SURFACE_SIDE_STYLE ('',( #5630 ) ) ;
#7651 = PRESENTATION_LAYER_ASSIGNMENT (  '', '', ( #15898 ) ) ;
#7652 = ORIENTED_EDGE ( 'NONE', *, *, #14573, .F. ) ;
#7653 = EDGE_CURVE ( 'NONE', #18104, #18073, #6102, .T. ) ;
#7654 = CARTESIAN_POINT ( 'NONE',  ( -35.00000000000000000, 8.000000000000000000, -21.00000000000000000 ) ) ;
#7655 = FILL_AREA_STYLE ('',( #7767 ) ) ;
#7656 = ORIENTED_EDGE ( 'NONE', *, *, #16009, .T. ) ;
#7657 = FILL_AREA_STYLE ('',( #1328 ) ) ;
#7658 = DIRECTION ( 'NONE',  ( 1.000000000000000000, 0.000000000000000000, 0.000000000000000000 ) ) ;
#7659 = ORIENTED_EDGE ( 'NONE', *, *, #9456, .T. ) ;
#7660 = CARTESIAN_POINT ( 'NONE',  ( 18.99999999999998224, 10.00000000000000000, -39.99999999999999289 ) ) ;
#7661 = AXIS2_PLACEMENT_3D ( 'NONE', #1888, #12957, #9843 ) ;
#7662 = AXIS2_PLACEMENT_3D ( 'NONE', #11781, #9925, #13231 ) ;
#7663 = LINE ( 'NONE', #9196, #16290 ) ;
#7664 = SURFACE_STYLE_USAGE ( .BOTH. , #1459 ) ;
#7665 = CARTESIAN_POINT ( 'NONE',  ( 111.4893729001366012, 209.4935875941501422, 345.2279431939882670 ) ) ;
#7666 = ORIENTED_EDGE ( 'NONE', *, *, #8002, .F. ) ;
#7667 = CARTESIAN_POINT ( 'NONE',  ( 0.000000000000000000, 376.0487089519837127, -150.0000000000033538 ) ) ;
#7668 = ORIENTED_EDGE ( 'NONE', *, *, #11280, .T. ) ;
#7669 = CARTESIAN_POINT ( 'NONE',  ( -36.00000000000000711, 6.000000000000000000, -22.00000000000000355 ) ) ;
#7670 = VECTOR ( 'NONE', #19634, 1000.000000000000000 ) ;
#7671 = MECHANICAL_DESIGN_GEOMETRIC_PRESENTATION_REPRESENTATION (  '', ( #16889 ), #17871 ) ;
#7672 = PLANE ( 'NONE',  #12986 ) ;
#7673 = ORIENTED_EDGE ( 'NONE', *, *, #17310, .T. ) ;
#7674 = FACE_OUTER_BOUND ( 'NONE', #147, .T. ) ;
#7675 = VERTEX_POINT ( 'NONE', #1210 ) ;
#7676 = VERTEX_POINT ( 'NONE', #7538 ) ;
#7677 = CLOSED_SHELL ( 'NONE', ( #11727, #7497, #5195, #13264, #13314, #11143, #19416, #9636, #18190, #5860, #7166, #20086, #7173, #13945, #18489, #18974, #18160, #560, #15070, #10384, #10458, #14292, #5867, #7136, #16279, #3105, #19063, #11508, #6620, #13794, #16836, #8718, #1198, #8269 ) ) ;
#7678 = VERTEX_POINT ( 'NONE', #12383 ) ;
#7679 = CARTESIAN_POINT ( 'NONE',  ( 0.000000000000000000, 0.000000000000000000, -150.0000000000000000 ) ) ;
#7680 = ORIENTED_EDGE ( 'NONE', *, *, #18968, .F. ) ;
#7681 = CARTESIAN_POINT ( 'NONE',  ( 498.8117674897343932, 191.8198460455371333, 168.2339398819845826 ) ) ;
#7682 = VECTOR ( 'NONE', #3971, 1000.000000000000000 ) ;
#7683 = DIRECTION ( 'NONE',  ( -1.000000000000000000, 0.000000000000000000, 0.000000000000000000 ) ) ;
#7684 = PRESENTATION_STYLE_ASSIGNMENT (( #151 ) ) ;
#7685 = CARTESIAN_POINT ( 'NONE',  ( 0.000000000000000000, -3.000000000000000000, 0.000000000000000000 ) ) ;
#7686 = CARTESIAN_POINT ( 'NONE',  ( -211.5106270998635409, 113.1299228374912502, 29.36128450348865471 ) ) ;
#7687 = DIRECTION ( 'NONE',  ( 1.000000000000000000, 0.000000000000000000, 0.000000000000000000 ) ) ;
#7688 = DIRECTION ( 'NONE',  ( 1.000000000000000000, 0.000000000000000000, -0.000000000000000000 ) ) ;
#7689 = EDGE_CURVE ( 'NONE', #12429, #566, #9924, .T. ) ;
#7690 = FILL_AREA_STYLE_COLOUR ( '', #4414 ) ;
#7691 = COLOUR_RGB ( '', 0.08235294, 0.09019608, 0.10196078) ;
#7692 = AXIS2_PLACEMENT_3D ( 'NONE', #11715, #2106, #3574 ) ;
#7693 = FACE_OUTER_BOUND ( 'NONE', #3793, .T. ) ;
#7694 = DIRECTION ( 'NONE',  ( 1.000000000000000000, -0.000000000000000000, -0.000000000000000000 ) ) ;
#7695 = CARTESIAN_POINT ( 'NONE',  ( -40.00000000000000711, 0.000000000000000000, -26.00000000000000000 ) ) ;
#7696 =( NAMED_UNIT ( * ) PLANE_ANGLE_UNIT ( ) SI_UNIT ( $, .RADIAN. ) );
#7697 = DIRECTION ( 'NONE',  ( -0.000000000000000000, -1.000000000000000000, 0.000000000000000000 ) ) ;
#7698 = CARTESIAN_POINT ( 'NONE',  ( 1.399999999999999911, 0.000000000000000000, 0.000000000000000000 ) ) ;
#7699 = SURFACE_STYLE_FILL_AREA ( #10582 ) ;
#7700 =( NAMED_UNIT ( * ) PLANE_ANGLE_UNIT ( ) SI_UNIT ( $, .RADIAN. ) );
#7701 = EDGE_LOOP ( 'NONE', ( #3048, #1299, #8082, #12316 ) ) ;
#7702 = CIRCLE ( 'NONE', #4748, 10.00000000000000888 ) ;
#7703 = COLOUR_RGB ( '', 0.40784314, 0.44705882, 0.49803922) ;
#7704 =( GEOMETRIC_REPRESENTATION_CONTEXT ( 3 ) GLOBAL_UNCERTAINTY_ASSIGNED_CONTEXT ( ( #3923 ) ) GLOBAL_UNIT_ASSIGNED_CONTEXT ( ( #15280, #9098, #20098 ) ) REPRESENTATION_CONTEXT ( 'NONE', 'WORKASPACE' ) );
#7705 = VERTEX_POINT ( 'NONE', #302 ) ;
#7706 = PRESENTATION_LAYER_ASSIGNMENT (  '', '', ( #11651 ) ) ;
#7707 = VECTOR ( 'NONE', #13884, 1000.000000000000000 ) ;
#7708 = ORIENTED_EDGE ( 'NONE', *, *, #16960, .F. ) ;
#7709 = DIRECTION ( 'NONE',  ( 0.000000000000000000, 0.000000000000000000, -1.000000000000000000 ) ) ;
#7710 = EDGE_CURVE ( 'NONE', #2115, #198, #15785, .T. ) ;
#7711 = VECTOR ( 'NONE', #348, 1000.000000000000000 ) ;
#7712 = ORIENTED_EDGE ( 'NONE', *, *, #19202, .F. ) ;
#7713 = FACE_OUTER_BOUND ( 'NONE', #15742, .T. ) ;
#7714 = ORIENTED_EDGE ( 'NONE', *, *, #1797, .F. ) ;
#7715 = COLOUR_RGB ( '', 0.09019608, 0.27058824, 0.51372549) ;
#7716 = AXIS2_PLACEMENT_3D ( 'NONE', #9099, #7548, #6000 ) ;
#7717 = FILL_AREA_STYLE ('',( #1391 ) ) ;
#7718 =( NAMED_UNIT ( * ) PLANE_ANGLE_UNIT ( ) SI_UNIT ( $, .RADIAN. ) );
#7719 = DIRECTION ( 'NONE',  ( 0.000000000000000000, 0.000000000000000000, -1.000000000000000000 ) ) ;
#7720 = CARTESIAN_POINT ( 'NONE',  ( -2.980268877975830399, 60.39571231257155404, 9.020512128682495856 ) ) ;
#7721 = CARTESIAN_POINT ( 'NONE',  ( 498.8117674897343932, 191.8198460455371333, 71.76606011801538898 ) ) ;
#7722 = CARTESIAN_POINT ( 'NONE',  ( 143.0892156028631348, 80.91625508013694912, 245.0000000000000000 ) ) ;
#7723 = MECHANICAL_DESIGN_GEOMETRIC_PRESENTATION_REPRESENTATION (  '', ( #8397 ), #9689 ) ;
#7724 = EDGE_CURVE ( 'NONE', #16657, #5094, #6203, .T. ) ;
#7725 = MECHANICAL_DESIGN_GEOMETRIC_PRESENTATION_REPRESENTATION (  '', ( #8712 ), #4774 ) ;
#7726 = LINE ( 'NONE', #18941, #16510 ) ;
#7727 = CARTESIAN_POINT ( 'NONE',  ( 0.000000000000000000, 368.2663108437010919, -142.2176018917206761 ) ) ;
#7728 = VECTOR ( 'NONE', #531, 1000.000000000000000 ) ;
#7729 = EDGE_CURVE ( 'NONE', #2260, #13941, #363, .T. ) ;
#7730 = ORIENTED_EDGE ( 'NONE', *, *, #9788, .T. ) ;
#7731 = PRESENTATION_LAYER_ASSIGNMENT (  '', '', ( #16640 ) ) ;
#7732 = ORIENTED_EDGE ( 'NONE', *, *, #300, .T. ) ;
#7733 = AXIS2_PLACEMENT_3D ( 'NONE', #20137, #6046, #15747 ) ;
#7734 = CARTESIAN_POINT ( 'NONE',  ( 423.8334540492694487, 191.8198460455371333, 158.2339398819845826 ) ) ;
#7735 = VERTEX_POINT ( 'NONE', #17319 ) ;
#7736 = ORIENTED_EDGE ( 'NONE', *, *, #11599, .F. ) ;
#7737 = ORIENTED_EDGE ( 'NONE', *, *, #16919, .F. ) ;
#7738 = CARTESIAN_POINT ( 'NONE',  ( 458.8334540492693350, 0.000000000000000000, 0.000000000000000000 ) ) ;
#7739 = COLOUR_RGB ( '', 0.08235294, 0.09019608, 0.10196078) ;
#7740 = CARTESIAN_POINT ( 'NONE',  ( 55.48937290013659407, 211.0574367717017594, 346.4752554294135507 ) ) ;
#7741 = VECTOR ( 'NONE', #9744, 1000.000000000000000 ) ;
#7742 = ADVANCED_FACE ( 'NONE', ( #14217 ), #12477, .F. ) ;
#7743 = SURFACE_STYLE_USAGE ( .BOTH. , #9087 ) ;
#7744 = SURFACE_STYLE_USAGE ( .BOTH. , #7539 ) ;
#7745 = ORIENTED_EDGE ( 'NONE', *, *, #11745, .F. ) ;
#7746 = DIRECTION ( 'NONE',  ( 0.000000000000000000, 1.000000000000000000, 0.000000000000000000 ) ) ;
#7747 = DIRECTION ( 'NONE',  ( -1.000000000000000000, -0.000000000000000000, -8.673617379884027583E-16 ) ) ;
#7748 = VECTOR ( 'NONE', #20260, 1000.000000000000000 ) ;
#7749 = PLANE ( 'NONE',  #143 ) ;
#7750 = CARTESIAN_POINT ( 'NONE',  ( 423.8334540492694487, 191.8198460455371333, 24.99421986894476078 ) ) ;
#7751 = DIRECTION ( 'NONE',  ( 1.000000000000000000, 0.000000000000000000, -0.000000000000000000 ) ) ;
#7752 = AXIS2_PLACEMENT_3D ( 'NONE', #9111, #7363, #15400 ) ;
#7753 = EDGE_CURVE ( 'NONE', #13610, #15622, #2000, .T. ) ;
#7754 = VERTEX_POINT ( 'NONE', #9794 ) ;
#7755 = CARTESIAN_POINT ( 'NONE',  ( -37.00000000000000000, 68.00000000000000000, -22.99999999999999645 ) ) ;
#7756 = CARTESIAN_POINT ( 'NONE',  ( 88.88953019741013861, 167.9162550801369491, 245.0000000000000000 ) ) ;
#7757 = DIRECTION ( 'NONE',  ( 0.000000000000000000, 0.000000000000000000, -1.000000000000000000 ) ) ;
#7758 = VECTOR ( 'NONE', #22, 1000.000000000000000 ) ;
#7759 = EDGE_CURVE ( 'NONE', #530, #10424, #12577, .T. ) ;
#7760 =( GEOMETRIC_REPRESENTATION_CONTEXT ( 3 ) GLOBAL_UNCERTAINTY_ASSIGNED_CONTEXT ( ( #19032 ) ) GLOBAL_UNIT_ASSIGNED_CONTEXT ( ( #13935, #12402, #2898 ) ) REPRESENTATION_CONTEXT ( 'NONE', 'WORKASPACE' ) );
#7761 = EDGE_CURVE ( 'NONE', #13085, #15933, #6638, .T. ) ;
#7762 = ORIENTED_EDGE ( 'NONE', *, *, #385, .T. ) ;
#7763 = EDGE_CURVE ( 'NONE', #8487, #7477, #1732, .T. ) ;
#7764 = ORIENTED_EDGE ( 'NONE', *, *, #2630, .T. ) ;
#7765 = EDGE_CURVE ( 'NONE', #1468, #14969, #6717, .T. ) ;
#7766 = PRESENTATION_STYLE_ASSIGNMENT (( #4975 ) ) ;
#7767 = FILL_AREA_STYLE_COLOUR ( '', #19723 ) ;
#7768 = ORIENTED_EDGE ( 'NONE', *, *, #9990, .F. ) ;
#7769 = CARTESIAN_POINT ( 'NONE',  ( -81.18192946989242387, 216.7545334744432921, 490.5655098179833544 ) ) ;
#7770 =( NAMED_UNIT ( * ) SI_UNIT ( $, .STERADIAN. ) SOLID_ANGLE_UNIT ( ) );
#7771 =( GEOMETRIC_REPRESENTATION_CONTEXT ( 3 ) GLOBAL_UNCERTAINTY_ASSIGNED_CONTEXT ( ( #2060 ) ) GLOBAL_UNIT_ASSIGNED_CONTEXT ( ( #15267, #2681, #18656 ) ) REPRESENTATION_CONTEXT ( 'NONE', 'WORKASPACE' ) );
#7772 = SURFACE_STYLE_FILL_AREA ( #9195 ) ;
#7773 = VECTOR ( 'NONE', #8488, 1000.000000000000000 ) ;
#7774 = CARTESIAN_POINT ( 'NONE',  ( 0.8562747324767706614, 140.4115240776867495, 500.8315376115346567 ) ) ;
#7775 = CARTESIAN_POINT ( 'NONE',  ( 498.8334540492693918, 191.8198460455371333, 158.2339398819845826 ) ) ;
#7776 = FACE_OUTER_BOUND ( 'NONE', #13377, .T. ) ;
#7777 = ORIENTED_EDGE ( 'NONE', *, *, #11378, .T. ) ;
#7778 = CARTESIAN_POINT ( 'NONE',  ( -31.00000000000000000, 11.00000000000000000, -31.00000000000000000 ) ) ;
#7779 = DIRECTION ( 'NONE',  ( 0.000000000000000000, 0.000000000000000000, 1.000000000000000000 ) ) ;
#7780 = CARTESIAN_POINT ( 'NONE',  ( -20.99999999999999645, 19.00000000000000000, 31.00000000000003197 ) ) ;
#7781 = SHAPE_DEFINITION_REPRESENTATION ( #1659, #10380 ) ;
#7782 = PRODUCT_DEFINITION_SHAPE ( 'NONE', 'NONE',  #9349 ) ;
#7783 = ORIENTED_EDGE ( 'NONE', *, *, #3415, .F. ) ;
#7784 = CARTESIAN_POINT ( 'NONE',  ( 53.48937290013659407, 127.7247684487574304, 250.0000000000000000 ) ) ;
#7785 = ORIENTED_EDGE ( 'NONE', *, *, #16182, .T. ) ;
#7786 = ORIENTED_EDGE ( 'NONE', *, *, #1277, .F. ) ;
#7787 = VECTOR ( 'NONE', #18520, 1000.000000000000000 ) ;
#7788 = VERTEX_POINT ( 'NONE', #10937 ) ;
#7789 = EDGE_CURVE ( 'NONE', #6058, #11555, #4950, .T. ) ;
#7790 = VECTOR ( 'NONE', #1699, 1000.000000000000000 ) ;
#7791 = EDGE_CURVE ( 'NONE', #4190, #19679, #1400, .T. ) ;
#7792 = VERTEX_POINT ( 'NONE', #11333 ) ;
#7793 = DIRECTION ( 'NONE',  ( 0.000000000000000000, 0.000000000000000000, -1.000000000000000000 ) ) ;
#7794 = EDGE_CURVE ( 'NONE', #9566, #13692, #3516, .T. ) ;
#7795 = FILL_AREA_STYLE ('',( #1475 ) ) ;
#7796 = CARTESIAN_POINT ( 'NONE',  ( -80.10887714076795874, 139.9048413501793391, 489.0362475460869973 ) ) ;
#7797 =( LENGTH_UNIT ( ) NAMED_UNIT ( * ) SI_UNIT ( .MILLI., .METRE. ) );
#7798 = CYLINDRICAL_SURFACE ( 'NONE', #10492, 10.00000000000000888 ) ;
#7799 = FILL_AREA_STYLE ('',( #7690 ) ) ;
#7800 = ORIENTED_EDGE ( 'NONE', *, *, #12255, .F. ) ;
#7801 = DIRECTION ( 'NONE',  ( -0.000000000000000000, -0.000000000000000000, 1.000000000000000000 ) ) ;
#7802 = CARTESIAN_POINT ( 'NONE',  ( -40.00000000000000000, 68.00000000000000000, 26.00000000000000355 ) ) ;
#7803 = DIRECTION ( 'NONE',  ( -0.000000000000000000, -1.000000000000000000, -0.000000000000000000 ) ) ;
#7804 = VECTOR ( 'NONE', #10072, 1000.000000000000000 ) ;
#7805 = CARTESIAN_POINT ( 'NONE',  ( -40.00000000000000711, 6.000000000000000000, -18.00000000000000355 ) ) ;
#7806 = CARTESIAN_POINT ( 'NONE',  ( 498.8117674897343932, 214.2156642432025251, 0.000000000000000000 ) ) ;
#7807 = FILL_AREA_STYLE_COLOUR ( '', #13240 ) ;
#7808 = ORIENTED_EDGE ( 'NONE', *, *, #1925, .T. ) ;
#7809 = ORIENTED_EDGE ( 'NONE', *, *, #16906, .F. ) ;
#7810 = VERTEX_POINT ( 'NONE', #6712 ) ;
#7811 = EDGE_CURVE ( 'NONE', #13581, #12734, #19356, .T. ) ;
#7812 = EDGE_LOOP ( 'NONE', ( #8451, #2083 ) ) ;
#7813 = CARTESIAN_POINT ( 'NONE',  ( 0.000000000000000000, 0.000000000000000000, 495.1946179577816451 ) ) ;
#7814 = FACE_OUTER_BOUND ( 'NONE', #3750, .T. ) ;
#7815 = VERTEX_POINT ( 'NONE', #17720 ) ;
#7816 =( NAMED_UNIT ( * ) SI_UNIT ( $, .STERADIAN. ) SOLID_ANGLE_UNIT ( ) );
#7817 = EDGE_LOOP ( 'NONE', ( #17943, #18481, #2415, #17382 ) ) ;
#7818 =( NAMED_UNIT ( * ) SI_UNIT ( $, .STERADIAN. ) SOLID_ANGLE_UNIT ( ) );
#7819 = DIRECTION ( 'NONE',  ( -1.000000000000000000, 0.000000000000000000, -0.000000000000000000 ) ) ;
#7820 = CARTESIAN_POINT ( 'NONE',  ( -2.257948793614859451, 61.98480561674775657, 9.228844315538689003 ) ) ;
#7821 =( NAMED_UNIT ( * ) SI_UNIT ( $, .STERADIAN. ) SOLID_ANGLE_UNIT ( ) );
#7822 = DIRECTION ( 'NONE',  ( 3.854941057726249930E-16, 0.000000000000000000, -1.000000000000000000 ) ) ;
#7823 = CARTESIAN_POINT ( 'NONE',  ( 34.00000000000002842, 3.000000000000000000, 23.00000000000000355 ) ) ;
#7824 = CARTESIAN_POINT ( 'NONE',  ( 54.31780002488277148, 209.7811923590225547, 348.0151256184570343 ) ) ;
#7825 = VECTOR ( 'NONE', #8254, 1000.000000000000000 ) ;
#7826 = DIRECTION ( 'NONE',  ( -0.000000000000000000, -1.000000000000000000, 0.000000000000000000 ) ) ;
#7827 = LINE ( 'NONE', #18736, #19047 ) ;
#7828 = ORIENTED_EDGE ( 'NONE', *, *, #12142, .T. ) ;
#7829 = ORIENTED_EDGE ( 'NONE', *, *, #12284, .T. ) ;
#7830 = VERTEX_POINT ( 'NONE', #13411 ) ;
#7831 = ORIENTED_EDGE ( 'NONE', *, *, #11357, .F. ) ;
#7832 = VERTEX_POINT ( 'NONE', #699 ) ;
#7833 = ORIENTED_EDGE ( 'NONE', *, *, #3986, .T. ) ;
#7834 = DIRECTION ( 'NONE',  ( -1.000000000000000000, -9.815121534730717399E-17, 0.000000000000000000 ) ) ;
#7835 = CYLINDRICAL_SURFACE ( 'NONE', #3772, 3.883636366625808911 ) ;
#7836 = EDGE_CURVE ( 'NONE', #11398, #3506, #17815, .T. ) ;
#7837 = AXIS2_PLACEMENT_3D ( 'NONE', #3388, #4727, #11310 ) ;
#7838 = LINE ( 'NONE', #12698, #3496 ) ;
#7839 = PRODUCT_DEFINITION ( 'UNKNOWN', '', #16881, #2451 ) ;
#7840 = CARTESIAN_POINT ( 'NONE',  ( 0.000000000000000000, 381.0487089519826895, 2.719601036885452502E-12 ) ) ;
#7841 = FILL_AREA_STYLE_COLOUR ( '', #12667 ) ;
#7842 = FACE_BOUND ( 'NONE', #19228, .T. ) ;
#7843 =( NAMED_UNIT ( * ) PLANE_ANGLE_UNIT ( ) SI_UNIT ( $, .RADIAN. ) );
#7844 = ORIENTED_EDGE ( 'NONE', *, *, #2414, .T. ) ;
#7845 = CARTESIAN_POINT ( 'NONE',  ( 30.99999999999999645, 3.000000000000000000, -25.99999999999999645 ) ) ;
#7846 = EDGE_CURVE ( 'NONE', #17086, #4537, #4067, .T. ) ;
#7847 = DIRECTION ( 'NONE',  ( 1.000000000000000000, 5.889072920838430686E-16, -0.000000000000000000 ) ) ;
#7848 = STYLED_ITEM ( 'NONE', ( #3774 ), #4833 ) ;
#7849 = EDGE_LOOP ( 'NONE', ( #3739, #15198 ) ) ;
#7850 = ADVANCED_FACE ( 'NONE', ( #19646 ), #14635, .F. ) ;
#7851 = ADVANCED_FACE ( 'NONE', ( #18108, #19276, #2348, #11753, #604 ), #11441, .F. ) ;
#7852 = DIRECTION ( 'NONE',  ( 0.000000000000000000, 1.000000000000000000, 0.000000000000000000 ) ) ;
#7853 = EDGE_LOOP ( 'NONE', ( #1928, #2186, #953, #18457 ) ) ;
#7854 = FACE_OUTER_BOUND ( 'NONE', #19203, .T. ) ;
#7855 = CARTESIAN_POINT ( 'NONE',  ( 503.8334540492693918, 191.8198460455371333, 215.0057801310552179 ) ) ;
#7856 = ORIENTED_EDGE ( 'NONE', *, *, #11643, .T. ) ;
#7857 = DIRECTION ( 'NONE',  ( 0.000000000000000000, 0.000000000000000000, 1.000000000000000000 ) ) ;
#7858 = CYLINDRICAL_SURFACE ( 'NONE', #19569, 10.00000000000000888 ) ;
#7859 = EDGE_CURVE ( 'NONE', #13299, #10437, #9889, .T. ) ;
#7860 = PRESENTATION_LAYER_ASSIGNMENT (  '', '', ( #3609 ) ) ;
#7861 = CARTESIAN_POINT ( 'NONE',  ( 0.8155011883608258572, 139.7530151083513772, 500.8359591266525968 ) ) ;
#7862 = EDGE_CURVE ( 'NONE', #2696, #14745, #16493, .T. ) ;
#7863 = DIRECTION ( 'NONE',  ( 0.000000000000000000, -0.000000000000000000, -1.000000000000000000 ) ) ;
#7864 = CARTESIAN_POINT ( 'NONE',  ( 31.00000000000000000, 19.00000000000000000, 30.99999999999999289 ) ) ;
#7865 = LINE ( 'NONE', #17136, #10360 ) ;
#7866 = ORIENTED_EDGE ( 'NONE', *, *, #7729, .T. ) ;
#7867 = CARTESIAN_POINT ( 'NONE',  ( -81.18192946989275072, 216.7545334744432921, 500.8237260975782874 ) ) ;
#7868 = FACE_OUTER_BOUND ( 'NONE', #5459, .T. ) ;
#7869 = FILL_AREA_STYLE ('',( #18685 ) ) ;
#7870 = CONTEXT_DEPENDENT_SHAPE_REPRESENTATION ( #1675, #16044 ) ;
#7871 = ORIENTED_EDGE ( 'NONE', *, *, #4475, .F. ) ;
#7872 = VERTEX_POINT ( 'NONE', #511 ) ;
#7873 = EDGE_CURVE ( 'NONE', #18411, #19036, #3710, .T. ) ;
#7874 = VERTEX_POINT ( 'NONE', #9993 ) ;
#7875 = ORIENTED_EDGE ( 'NONE', *, *, #14201, .F. ) ;
#7876 = AXIS2_PLACEMENT_3D ( 'NONE', #7311, #15246, #13703 ) ;
#7877 = VECTOR ( 'NONE', #9181, 1000.000000000000000 ) ;
#7878 = ORIENTED_EDGE ( 'NONE', *, *, #1340, .T. ) ;
#7879 = CARTESIAN_POINT ( 'NONE',  ( 98.48937290013660117, 80.91625508013694912, -97.94896630388704750 ) ) ;
#7880 = ADVANCED_FACE ( 'NONE', ( #13113 ), #11639, .T. ) ;
#7881 = EDGE_LOOP ( 'NONE', ( #6029, #9376, #15763, #93 ) ) ;
#7882 = DIRECTION ( 'NONE',  ( 1.000000000000000000, 0.000000000000000000, 0.000000000000000000 ) ) ;
#7883 = DIRECTION ( 'NONE',  ( 0.000000000000000000, 0.000000000000000000, 1.000000000000000000 ) ) ;
#7884 = DIRECTION ( 'NONE',  ( 0.000000000000000000, 0.000000000000000000, 1.000000000000000000 ) ) ;
#7885 = VECTOR ( 'NONE', #5855, 1000.000000000000000 ) ;
#7886 = FACE_OUTER_BOUND ( 'NONE', #2280, .T. ) ;
#7887 = DIRECTION ( 'NONE',  ( -1.000000000000000000, 0.000000000000000000, 0.000000000000000000 ) ) ;
#7888 = AXIS2_PLACEMENT_3D ( 'NONE', #7685, #15328, #1251 ) ;
#7889 = SURFACE_STYLE_FILL_AREA ( #3253 ) ;
#7890 = VECTOR ( 'NONE', #5511, 1000.000000000000114 ) ;
#7891 = LINE ( 'NONE', #4389, #10664 ) ;
#7892 = ORIENTED_EDGE ( 'NONE', *, *, #5725, .F. ) ;
#7893 = DIRECTION ( 'NONE',  ( 0.000000000000000000, -1.000000000000000000, 0.000000000000000000 ) ) ;
#7894 = EDGE_CURVE ( 'NONE', #3463, #1029, #19554, .T. ) ;
#7895 = SURFACE_STYLE_USAGE ( .BOTH. , #18800 ) ;
#7896 = CARTESIAN_POINT ( 'NONE',  ( -25.99999999999999645, 68.00000000000000000, 31.00000000000003908 ) ) ;
#7897 = CARTESIAN_POINT ( 'NONE',  ( 31.00000000000003553, 19.00000000000000000, 25.99999999999999645 ) ) ;
#7898 = CARTESIAN_POINT ( 'NONE',  ( -37.00000000000000711, 0.000000000000000000, 23.00000000000000000 ) ) ;
#7899 = SURFACE_STYLE_FILL_AREA ( #1371 ) ;
#7900 = LINE ( 'NONE', #10892, #17770 ) ;
#7901 = ADVANCED_BREP_SHAPE_REPRESENTATION ( '', ( #1583, #2741 ), #19798 ) ;
#7902 = ORIENTED_EDGE ( 'NONE', *, *, #4472, .T. ) ;
#7903 = ADVANCED_FACE ( 'NONE', ( #20053 ), #19855, .F. ) ;
#7904 = ORIENTED_EDGE ( 'NONE', *, *, #7451, .T. ) ;
#7905 = DIRECTION ( 'NONE',  ( -0.000000000000000000, -1.000000000000000000, -0.000000000000000000 ) ) ;
#7906 =( GEOMETRIC_REPRESENTATION_CONTEXT ( 3 ) GLOBAL_UNCERTAINTY_ASSIGNED_CONTEXT ( ( #13027 ) ) GLOBAL_UNIT_ASSIGNED_CONTEXT ( ( #4934, #14011, #1286 ) ) REPRESENTATION_CONTEXT ( 'NONE', 'WORKASPACE' ) );
#7907 = AXIS2_PLACEMENT_3D ( 'NONE', #9627, #17366, #6352 ) ;
#7908 = VECTOR ( 'NONE', #8177, 1000.000000000000000 ) ;
#7909 = ORIENTED_EDGE ( 'NONE', *, *, #9758, .T. ) ;
#7910 = CARTESIAN_POINT ( 'NONE',  ( -79.34077595268365712, 139.9822134344571225, 501.2042671826797573 ) ) ;
#7911 = ORIENTED_EDGE ( 'NONE', *, *, #10396, .F. ) ;
#7912 = CARTESIAN_POINT ( 'NONE',  ( -79.99999999999995737, 138.7545334744432637, 489.5655098179848892 ) ) ;
#7913 = EDGE_CURVE ( 'NONE', #8713, #1949, #5868, .T. ) ;
#7914 = ORIENTED_EDGE ( 'NONE', *, *, #17944, .F. ) ;
#7915 = CARTESIAN_POINT ( 'NONE',  ( -64.99999999999995737, 317.7545334744432353, 495.1946179577816451 ) ) ;
#7916 =( NAMED_UNIT ( * ) SI_UNIT ( $, .STERADIAN. ) SOLID_ANGLE_UNIT ( ) );
#7917 =( NAMED_UNIT ( * ) SI_UNIT ( $, .STERADIAN. ) SOLID_ANGLE_UNIT ( ) );
#7918 = LINE ( 'NONE', #14309, #8484 ) ;
#7919 = CIRCLE ( 'NONE', #19419, 10.00000000000000178 ) ;
#7920 = LINE ( 'NONE', #1714, #14590 ) ;
#7921 = DIRECTION ( 'NONE',  ( 1.000000000000000000, 0.000000000000000000, 0.000000000000000000 ) ) ;
#7922 = COLOUR_RGB ( '', 0.31764706, 0.68627451, 0.89019608) ;
#7923 = DIRECTION ( 'NONE',  ( -0.000000000000000000, -1.000000000000000000, -0.000000000000000000 ) ) ;
#7924 = MECHANICAL_DESIGN_GEOMETRIC_PRESENTATION_REPRESENTATION (  '', ( #6289 ), #13208 ) ;
#7925 = DIRECTION ( 'NONE',  ( -1.000000000000000000, -9.815121534730717399E-17, 0.000000000000000000 ) ) ;
#7926 = LINE ( 'NONE', #14207, #12639 ) ;
#7927 = ORIENTED_EDGE ( 'NONE', *, *, #16834, .F. ) ;
#7928 = EDGE_LOOP ( 'NONE', ( #8195, #11055 ) ) ;
#7929 = UNCERTAINTY_MEASURE_WITH_UNIT (LENGTH_MEASURE( 1.000000000000000082E-05 ), #12701, 'distance_accuracy_value', 'NONE');
#7930 = LINE ( 'NONE', #2976, #4773 ) ;
#7931 = ORIENTED_EDGE ( 'NONE', *, *, #11994, .F. ) ;
#7932 = ORIENTED_EDGE ( 'NONE', *, *, #15550, .T. ) ;
#7933 = VERTEX_POINT ( 'NONE', #1186 ) ;
#7934 = CARTESIAN_POINT ( 'NONE',  ( -26.00000000000002842, 3.000000000000000000, -31.00000000000003197 ) ) ;
#7935 = VECTOR ( 'NONE', #904, 1000.000000000000000 ) ;
#7936 = AXIS2_PLACEMENT_3D ( 'NONE', #14349, #17230, #3118 ) ;
#7937 = CARTESIAN_POINT ( 'NONE',  ( -20.99999999999999645, 19.00000000000000000, -31.00000000000003908 ) ) ;
#7938 = CARTESIAN_POINT ( 'NONE',  ( -1.000000000000007550, 146.8256012863087676, 480.6843163258854474 ) ) ;
#7939 = LINE ( 'NONE', #6409, #18053 ) ;
#7940 = DIRECTION ( 'NONE',  ( -1.000000000000000000, 0.000000000000000000, -0.000000000000000000 ) ) ;
#7941 = PRODUCT ( 'Servo-Head', 'Servo-Head', '', ( #12828 ) ) ;
#7942 = FILL_AREA_STYLE_COLOUR ( '', #5432 ) ;
#7943 = LINE ( 'NONE', #11761, #20090 ) ;
#7944 = DIRECTION ( 'NONE',  ( 0.000000000000000000, 0.000000000000000000, -1.000000000000000000 ) ) ;
#7945 = EDGE_CURVE ( 'NONE', #10544, #6229, #7215, .T. ) ;
#7946 = EDGE_LOOP ( 'NONE', ( #14213, #2909, #12824, #1077 ) ) ;
#7947 = CARTESIAN_POINT ( 'NONE',  ( -81.18192946989243808, 138.7723821175108014, 490.5025619657601510 ) ) ;
#7948 = CARTESIAN_POINT ( 'NONE',  ( 0.3499999999999999778, 18.17500000000000071, 0.000000000000000000 ) ) ;
#7949 = VECTOR ( 'NONE', #5783, 1000.000000000000000 ) ;
#7950 = CIRCLE ( 'NONE', #2691, 3.000000000000000888 ) ;
#7951 = ORIENTED_EDGE ( 'NONE', *, *, #11567, .F. ) ;
#7952 = LINE ( 'NONE', #4659, #19754 ) ;
#7953 = EDGE_LOOP ( 'NONE', ( #8011, #11, #3630, #19091, #17526, #6816, #2079, #17232 ) ) ;
#7954 = EDGE_CURVE ( 'NONE', #5834, #10863, #18516, .T. ) ;
#7955 = CARTESIAN_POINT ( 'NONE',  ( 98.48937290013662960, 103.1299228374914208, 170.4174721992565082 ) ) ;
#7956 = STYLED_ITEM ( 'NONE', ( #11935 ), #17542 ) ;
#7957 = CARTESIAN_POINT ( 'NONE',  ( 468.8334540492694487, 214.2156642432025251, 250.0000000000000000 ) ) ;
#7958 = ORIENTED_EDGE ( 'NONE', *, *, #12033, .F. ) ;
#7959 = DIRECTION ( 'NONE',  ( -0.000000000000000000, -0.000000000000000000, 1.000000000000000000 ) ) ;
#7960 = CARTESIAN_POINT ( 'NONE',  ( 463.8334540492693350, 191.8198460455371333, 158.2339398819845826 ) ) ;
#7961 = VECTOR ( 'NONE', #7096, 1000.000000000000000 ) ;
#7962 = CARTESIAN_POINT ( 'NONE',  ( -0.7871933770022689902, 140.1302042697082300, 501.4486251228268543 ) ) ;
#7963 = DIRECTION ( 'NONE',  ( 1.000000000000000000, 0.000000000000000000, 1.135258727068399668E-15 ) ) ;
#7964 = CARTESIAN_POINT ( 'NONE',  ( 22.99999999999998224, 0.000000000000000000, 37.00000000000000711 ) ) ;
#7965 = DIRECTION ( 'NONE',  ( 1.000000000000000000, 5.889072920838430686E-16, -0.000000000000000000 ) ) ;
#7966 = VECTOR ( 'NONE', #1599, 1000.000000000000000 ) ;
#7967 = ORIENTED_EDGE ( 'NONE', *, *, #6657, .T. ) ;
#7968 = DIRECTION ( 'NONE',  ( 0.000000000000000000, 1.000000000000000000, 0.000000000000000000 ) ) ;
#7969 = EDGE_CURVE ( 'NONE', #4687, #6099, #8853, .T. ) ;
#7970 = VERTEX_POINT ( 'NONE', #1087 ) ;
#7971 = DIRECTION ( 'NONE',  ( 1.000000000000000000, 0.000000000000000000, 0.000000000000000000 ) ) ;
#7972 = ORIENTED_EDGE ( 'NONE', *, *, #4171, .F. ) ;
#7973 = CIRCLE ( 'NONE', #9954, 10.00000000000000888 ) ;
#7974 = STYLED_ITEM ( 'NONE', ( #16963 ), #17786 ) ;
#7975 = ORIENTED_EDGE ( 'NONE', *, *, #4353, .F. ) ;
#7976 = EDGE_CURVE ( 'NONE', #10796, #19149, #10405, .T. ) ;
#7977 = EDGE_LOOP ( 'NONE', ( #7089, #4431, #15638, #13671 ) ) ;
#7978 = CARTESIAN_POINT ( 'NONE',  ( 493.8117674897343363, 214.2156642432025251, 245.0000000000000000 ) ) ;
#7979 = ORIENTED_EDGE ( 'NONE', *, *, #13931, .F. ) ;
#7980 = CIRCLE ( 'NONE', #6002, 10.00000000000000888 ) ;
#7981 = VERTEX_POINT ( 'NONE', #12065 ) ;
#7982 = STYLED_ITEM ( 'NONE', ( #12390 ), #11689 ) ;
#7983 = DIRECTION ( 'NONE',  ( 0.000000000000000000, 0.000000000000000000, -1.000000000000000000 ) ) ;
#7984 = CARTESIAN_POINT ( 'NONE',  ( 3.850000000000000089, 0.000000000000000000, 0.000000000000000000 ) ) ;
#7985 = ORIENTED_EDGE ( 'NONE', *, *, #8535, .F. ) ;
#7986 = EDGE_CURVE ( 'NONE', #15133, #18411, #766, .T. ) ;
#7987 = ADVANCED_FACE ( 'NONE', ( #7422 ), #2657, .F. ) ;
#7988 =( NAMED_UNIT ( * ) PLANE_ANGLE_UNIT ( ) SI_UNIT ( $, .RADIAN. ) );
#7989 = CIRCLE ( 'NONE', #9982, 1.000000000000015987 ) ;
#7990 = DIRECTION ( 'NONE',  ( 1.000000000000000000, 5.889072920838430686E-16, -0.000000000000000000 ) ) ;
#7991 = SURFACE_STYLE_FILL_AREA ( #8205 ) ;
#7992 = CARTESIAN_POINT ( 'NONE',  ( -78.99999999999995737, 147.7545334744432921, 496.6642397995874489 ) ) ;
#7993 = DIRECTION ( 'NONE',  ( 0.000000000000000000, 1.000000000000000000, 0.000000000000000000 ) ) ;
#7994 = VECTOR ( 'NONE', #5315, 1000.000000000000000 ) ;
#7995 = EDGE_LOOP ( 'NONE', ( #1269, #15349 ) ) ;
#7996 = DIRECTION ( 'NONE',  ( 0.000000000000000000, 1.000000000000000000, 0.000000000000000000 ) ) ;
#7997 = CARTESIAN_POINT ( 'NONE',  ( -40.00000000000000000, 68.00000000000000000, -25.99999999999999645 ) ) ;
#7998 = CARTESIAN_POINT ( 'NONE',  ( 98.48937290013662960, 113.1299228374914350, 29.36128450348865471 ) ) ;
#7999 = DIRECTION ( 'NONE',  ( -0.000000000000000000, -1.000000000000000000, -0.000000000000000000 ) ) ;
#8000 = SURFACE_STYLE_USAGE ( .BOTH. , #15654 ) ;
#8001 = FACE_BOUND ( 'NONE', #13490, .T. ) ;
#8002 = EDGE_CURVE ( 'NONE', #18751, #7513, #12238, .T. ) ;
#8003 = AXIS2_PLACEMENT_3D ( 'NONE', #6354, #18906, #4809 ) ;
#8004 = DIRECTION ( 'NONE',  ( 1.000000000000000000, 8.344193210541727648E-14, -1.322943490866811299E-12 ) ) ;
#8005 = DIRECTION ( 'NONE',  ( 0.000000000000000000, 0.000000000000000000, -1.000000000000000000 ) ) ;
#8006 = ORIENTED_EDGE ( 'NONE', *, *, #18614, .F. ) ;
#8007 = ORIENTED_EDGE ( 'NONE', *, *, #9904, .F. ) ;
#8008 = DIRECTION ( 'NONE',  ( -1.000000000000000000, 0.000000000000000000, -0.000000000000000000 ) ) ;
#8009 = AXIS2_PLACEMENT_3D ( 'NONE', #1008, #11877, #8972 ) ;
#8010 = ADVANCED_FACE ( 'NONE', ( #10704 ), #16708, .F. ) ;
#8011 = ORIENTED_EDGE ( 'NONE', *, *, #598, .T. ) ;
#8012 = DIRECTION ( 'NONE',  ( -1.000000000000000000, 0.000000000000000000, -0.000000000000000000 ) ) ;
#8013 = DIRECTION ( 'NONE',  ( 0.000000000000000000, 1.000000000000000000, 0.000000000000000000 ) ) ;
#8014 = ORIENTED_EDGE ( 'NONE', *, *, #5716, .T. ) ;
#8015 = DIRECTION ( 'NONE',  ( 0.000000000000000000, 1.000000000000000000, 0.000000000000000000 ) ) ;
#8016 = CARTESIAN_POINT ( 'NONE',  ( -23.00000000000002487, 10.00000000000000000, -36.99999999999999289 ) ) ;
#8017 = CLOSED_SHELL ( 'NONE', ( #14410, #18434, #12872, #15094 ) ) ;
#8018 = AXIS2_PLACEMENT_3D ( 'NONE', #8544, #4137, #901 ) ;
#8019 = ORIENTED_EDGE ( 'NONE', *, *, #12147, .T. ) ;
#8020 = FACE_OUTER_BOUND ( 'NONE', #14051, .T. ) ;
#8021 = LINE ( 'NONE', #14501, #7966 ) ;
#8022 = DIRECTION ( 'NONE',  ( -0.000000000000000000, -0.000000000000000000, 1.000000000000000000 ) ) ;
#8023 = CARTESIAN_POINT ( 'NONE',  ( 40.00000000000001421, 5.000000000000000888, -150.0000000000000000 ) ) ;
#8024 = AXIS2_PLACEMENT_3D ( 'NONE', #17898, #3800, #492 ) ;
#8025 = STYLED_ITEM ( 'NONE', ( #9850 ), #18911 ) ;
#8026 = CARTESIAN_POINT ( 'NONE',  ( 34.99999999999997868, 11.00000000000000000, -40.00000000000000711 ) ) ;
#8027 = CARTESIAN_POINT ( 'NONE',  ( -1.000000000000000888, 146.1184945051221575, 507.7561228916242158 ) ) ;
#8028 = DIRECTION ( 'NONE',  ( -0.000000000000000000, -1.000000000000000000, -0.000000000000000000 ) ) ;
#8029 = DIRECTION ( 'NONE',  ( -1.000000000000000000, -0.000000000000000000, -1.135258727068399668E-15 ) ) ;
#8030 = PLANE ( 'NONE',  #6911 ) ;
#8031 = EDGE_CURVE ( 'NONE', #13058, #5525, #11106, .T. ) ;
#8032 = VERTEX_POINT ( 'NONE', #18724 ) ;
#8033 = AXIS2_PLACEMENT_3D ( 'NONE', #14377, #1569, #7983 ) ;
#8034 = EDGE_LOOP ( 'NONE', ( #11353, #6585, #17476, #1324 ) ) ;
#8035 = PRESENTATION_STYLE_ASSIGNMENT (( #11324 ) ) ;
#8036 = ORIENTED_EDGE ( 'NONE', *, *, #12152, .F. ) ;
#8037 = ADVANCED_FACE ( 'NONE', ( #9246 ), #182, .F. ) ;
#8038 = COLOUR_RGB ( '', 0.72549020, 0.75294118, 0.79215686) ;
#8039 = ORIENTED_EDGE ( 'NONE', *, *, #14743, .F. ) ;
#8040 = CARTESIAN_POINT ( 'NONE',  ( -25.99999999999999645, 68.00000000000000000, 40.00000000000002132 ) ) ;
#8041 =( GEOMETRIC_REPRESENTATION_CONTEXT ( 3 ) GLOBAL_UNCERTAINTY_ASSIGNED_CONTEXT ( ( #13032 ) ) GLOBAL_UNIT_ASSIGNED_CONTEXT ( ( #3743, #16232, #13230 ) ) REPRESENTATION_CONTEXT ( 'NONE', 'WORKASPACE' ) );
#8042 = DIRECTION ( 'NONE',  ( -0.000000000000000000, -0.000000000000000000, 1.000000000000000000 ) ) ;
#8043 = PRESENTATION_LAYER_ASSIGNMENT (  '', '', ( #3095 ) ) ;
#8044 = DIRECTION ( 'NONE',  ( 0.000000000000000000, 0.000000000000000000, -1.000000000000000000 ) ) ;
#8045 = DIRECTION ( 'NONE',  ( -0.000000000000000000, -1.000000000000000000, -0.000000000000000000 ) ) ;
#8046 = CARTESIAN_POINT ( 'NONE',  ( -31.00000000000003197, 19.00000000000000000, -26.00000000000000355 ) ) ;
#8047 = COLOUR_RGB ( '', 0.66274510, 0.83137255, 0.94901961) ;
#8048 =( LENGTH_UNIT ( ) NAMED_UNIT ( * ) SI_UNIT ( .MILLI., .METRE. ) );
#8049 = DIRECTION ( 'NONE',  ( -0.000000000000000000, -0.7071067811865445751, -0.7071067811865504593 ) ) ;
#8050 = TOROIDAL_SURFACE ( 'NONE', #4425, 14.76997474683060041, 0.5250000000000000222 ) ;
#8051 = DIRECTION ( 'NONE',  ( 0.000000000000000000, 0.000000000000000000, -1.000000000000000000 ) ) ;
#8052 = CARTESIAN_POINT ( 'NONE',  ( -75.00000000000000000, 0.000000000000000000, 0.000000000000000000 ) ) ;
#8053 = CARTESIAN_POINT ( 'NONE',  ( 0.000000000000000000, 145.9162550801369491, 250.0000000000000000 ) ) ;
#8054 = FILL_AREA_STYLE ('',( #1741 ) ) ;
#8055 = EDGE_LOOP ( 'NONE', ( #6126, #19927 ) ) ;
#8056 = LINE ( 'NONE', #7756, #10031 ) ;
#8057 = VECTOR ( 'NONE', #15621, 1000.000000000000000 ) ;
#8058 = AXIS2_PLACEMENT_3D ( 'NONE', #13, #19056, #3210 ) ;
#8059 =( LENGTH_UNIT ( ) NAMED_UNIT ( * ) SI_UNIT ( .MILLI., .METRE. ) );
#8060 = AXIS2_PLACEMENT_3D ( 'NONE', #14529, #11341, #12906 ) ;
#8061 = AXIS2_PLACEMENT_3D ( 'NONE', #7133, #8259, #13122 ) ;
#8062 = AXIS2_PLACEMENT_3D ( 'NONE', #2729, #1157, #12210 ) ;
#8063 = VECTOR ( 'NONE', #16573, 1000.000000000000000 ) ;
#8064 = DIRECTION ( 'NONE',  ( 1.000000000000000000, 0.000000000000000000, 0.000000000000000000 ) ) ;
#8065 = EDGE_LOOP ( 'NONE', ( #17758, #4777, #13824, #16303 ) ) ;
#8066 = STYLED_ITEM ( 'NONE', ( #5636 ), #10842 ) ;
#8067 = ADVANCED_FACE ( 'NONE', ( #12553 ), #18816, .F. ) ;
#8068 = CARTESIAN_POINT ( 'NONE',  ( 31.99999999999998579, 10.00000000000000000, 25.99999999999999645 ) ) ;
#8069 = VERTEX_POINT ( 'NONE', #4718 ) ;
#8070 = SURFACE_STYLE_USAGE ( .BOTH. , #6124 ) ;
#8071 = VECTOR ( 'NONE', #15722, 1000.000000000000000 ) ;
#8072 = VERTEX_POINT ( 'NONE', #15670 ) ;
#8073 = FILL_AREA_STYLE_COLOUR ( '', #19866 ) ;
#8074 = AXIS2_PLACEMENT_3D ( 'NONE', #6779, #19406, #8417 ) ;
#8075 = CARTESIAN_POINT ( 'NONE',  ( 463.8334540492693350, 191.8198460455371333, 71.76606011801538898 ) ) ;
#8076 = CARTESIAN_POINT ( 'NONE',  ( -0.08067209305391118135, 139.6450463499541570, 500.5689801128370391 ) ) ;
#8077 = CARTESIAN_POINT ( 'NONE',  ( 458.8334540492693350, 191.8198460455371333, 235.0057801310552463 ) ) ;
#8078 = AXIS2_PLACEMENT_3D ( 'NONE', #17041, #13740, #10545 ) ;
#8079 = DIRECTION ( 'NONE',  ( -1.000000000000000000, -0.000000000000000000, -0.000000000000000000 ) ) ;
#8080 = CYLINDRICAL_SURFACE ( 'NONE', #12526, 1.000000000000000888 ) ;
#8081 = DIRECTION ( 'NONE',  ( 0.000000000000000000, 0.000000000000000000, -1.000000000000000000 ) ) ;
#8082 = ORIENTED_EDGE ( 'NONE', *, *, #6142, .F. ) ;
#8083 = FACE_BOUND ( 'NONE', #6234, .T. ) ;
#8084 = CARTESIAN_POINT ( 'NONE',  ( 0.000000000000000000, 38.00000000000000711, -5.741599279633704455E-16 ) ) ;
#8085 = LINE ( 'NONE', #10966, #12650 ) ;
#8086 = ITEM_DEFINED_TRANSFORMATION ( 'NONE', 'NONE', #8679,  #2741 ) ;
#8087 = COLOUR_RGB ( '', 0.09019608, 0.27058824, 0.51372549) ;
#8088 = ORIENTED_EDGE ( 'NONE', *, *, #18752, .T. ) ;
#8089 = LINE ( 'NONE', #340, #17494 ) ;
#8090 = VERTEX_POINT ( 'NONE', #9457 ) ;
#8091 = EDGE_CURVE ( 'NONE', #12278, #417, #4522, .T. ) ;
#8092 = VERTEX_POINT ( 'NONE', #15556 ) ;
#8093 = VERTEX_POINT ( 'NONE', #1595 ) ;
#8094 = TOROIDAL_SURFACE ( 'NONE', #5463, 8.000000000000000000, 1.000000000000000000 ) ;
#8095 = DIRECTION ( 'NONE',  ( 0.000000000000000000, 0.000000000000000000, -1.000000000000000000 ) ) ;
#8096 = PLANE ( 'NONE',  #2411 ) ;
#8097 = VERTEX_POINT ( 'NONE', #1386 ) ;
#8098 = CARTESIAN_POINT ( 'NONE',  ( 21.99999999999998224, 8.000000000000000000, -35.99999999999999289 ) ) ;
#8099 = DIRECTION ( 'NONE',  ( 0.000000000000000000, 0.000000000000000000, 1.000000000000000000 ) ) ;
#8100 = CIRCLE ( 'NONE', #18293, 9.500000000000000000 ) ;
#8101 = ORIENTED_EDGE ( 'NONE', *, *, #15710, .F. ) ;
#8102 = CARTESIAN_POINT ( 'NONE',  ( -31.00000000000000000, 8.000000000000000000, -31.00000000000000000 ) ) ;
#8103 = EDGE_CURVE ( 'NONE', #11785, #12469, #10907, .T. ) ;
#8104 = DIRECTION ( 'NONE',  ( 0.000000000000000000, 1.000000000000000000, 0.000000000000000000 ) ) ;
#8105 = FACE_BOUND ( 'NONE', #9565, .T. ) ;
#8106 = CARTESIAN_POINT ( 'NONE',  ( 0.000000000000000000, 0.000000000000000000, -135.0000000000000284 ) ) ;
#8107 = CARTESIAN_POINT ( 'NONE',  ( 1.181929469893224560, 140.4048636633015406, 499.8237260975781737 ) ) ;
#8108 = CARTESIAN_POINT ( 'NONE',  ( 10.00000000000000000, 372.8685141053783241, -146.8198051533979935 ) ) ;
#8109 = PRODUCT_DEFINITION ( 'UNKNOWN', '', #15243, #7207 ) ;
#8110 = ORIENTED_EDGE ( 'NONE', *, *, #10898, .T. ) ;
#8111 = DIRECTION ( 'NONE',  ( 1.000000000000000000, -0.000000000000000000, 0.000000000000000000 ) ) ;
#8112 = CARTESIAN_POINT ( 'NONE',  ( 110.6609457753904024, 209.7811923590225263, 348.0151256184569775 ) ) ;
#8113 = DIRECTION ( 'NONE',  ( -0.000000000000000000, 1.000000000000000000, -0.000000000000000000 ) ) ;
#8114 = LINE ( 'NONE', #16066, #14943 ) ;
#8115 = CARTESIAN_POINT ( 'NONE',  ( 53.48937290013658696, 123.1299228374914065, 29.36128450348865471 ) ) ;
#8116 = DIRECTION ( 'NONE',  ( -0.000000000000000000, 1.000000000000000000, -0.000000000000000000 ) ) ;
#8117 = TOROIDAL_SURFACE ( 'NONE', #18632, 14.27500000000000036, 0.6999999999999999556 ) ;
#8118 = PRESENTATION_STYLE_ASSIGNMENT (( #20263 ) ) ;
#8119 = ADVANCED_FACE ( 'NONE', ( #7713 ), #19016, .F. ) ;
#8120 = VERTEX_POINT ( 'NONE', #8130 ) ;
#8121 = FACE_OUTER_BOUND ( 'NONE', #4056, .T. ) ;
#8122 = EDGE_CURVE ( 'NONE', #2876, #3672, #14400, .T. ) ;
#8123 = PRODUCT_DEFINITION_SHAPE ( 'NONE', 'NONE',  #7839 ) ;
#8124 = ORIENTED_EDGE ( 'NONE', *, *, #1295, .T. ) ;
#8125 = SURFACE_STYLE_USAGE ( .BOTH. , #6796 ) ;
#8126 = CARTESIAN_POINT ( 'NONE',  ( 153.4893729001366864, 113.1299228374914634, 29.36128450348865471 ) ) ;
#8127 = ORIENTED_EDGE ( 'NONE', *, *, #13257, .T. ) ;
#8128 = CARTESIAN_POINT ( 'NONE',  ( -211.5106270998635409, 113.1299228374912502, 170.4174721992565082 ) ) ;
#8129 = EDGE_CURVE ( 'NONE', #6114, #7322, #13572, .T. ) ;
#8130 = CARTESIAN_POINT ( 'NONE',  ( 82.88953019741013861, 167.9162550801369491, 250.0000000000000000 ) ) ;
#8131 = EDGE_LOOP ( 'NONE', ( #19329, #5349, #10114, #8662, #6605, #1545, #6687, #7828 ) ) ;
#8132 = DIRECTION ( 'NONE',  ( 1.000000000000000000, 9.815121534730717399E-17, 0.000000000000000000 ) ) ;
#8133 = VECTOR ( 'NONE', #14709, 1000.000000000000000 ) ;
#8134 = DIRECTION ( 'NONE',  ( 1.000000000000000000, 0.000000000000000000, 3.854941057726246479E-16 ) ) ;
#8135 = MANIFOLD_SOLID_BREP ( 'Cut-Extrude2', #3401 ) ;
#8136 = EDGE_CURVE ( 'NONE', #10467, #17875, #16231, .T. ) ;
#8137 = CARTESIAN_POINT ( 'NONE',  ( 0.000000000000000000, 313.8311070602663904, -87.78239810828596035 ) ) ;
#8138 = DIRECTION ( 'NONE',  ( -0.000000000000000000, 1.000000000000000000, -0.000000000000000000 ) ) ;
#8139 = DIRECTION ( 'NONE',  ( 0.000000000000000000, 0.000000000000000000, 1.000000000000000000 ) ) ;
#8140 = EDGE_CURVE ( 'NONE', #9751, #19129, #10075, .T. ) ;
#8141 = DIRECTION ( 'NONE',  ( 1.000000000000000000, 0.000000000000000000, 0.000000000000000000 ) ) ;
#8142 = CARTESIAN_POINT ( 'NONE',  ( 53.48937290013658696, 113.1299228374914065, 220.6387154965113382 ) ) ;
#8143 = FACE_OUTER_BOUND ( 'NONE', #9102, .T. ) ;
#8144 = ORIENTED_EDGE ( 'NONE', *, *, #19626, .T. ) ;
#8145 = EDGE_CURVE ( 'NONE', #7810, #10259, #9866, .T. ) ;
#8146 = EDGE_CURVE ( 'NONE', #1021, #13927, #4021, .T. ) ;
#8147 = VERTEX_POINT ( 'NONE', #14804 ) ;
#8148 = ORIENTED_EDGE ( 'NONE', *, *, #16934, .F. ) ;
#8149 = UNCERTAINTY_MEASURE_WITH_UNIT (LENGTH_MEASURE( 1.000000000000000082E-05 ), #16682, 'distance_accuracy_value', 'NONE');
#8150 = LINE ( 'NONE', #12787, #13974 ) ;
#8151 = ORIENTED_EDGE ( 'NONE', *, *, #11251, .T. ) ;
#8152 = ORIENTED_EDGE ( 'NONE', *, *, #17321, .F. ) ;
#8153 = CARTESIAN_POINT ( 'NONE',  ( 153.4893729001366864, 113.1299228374914634, 170.4174721992565082 ) ) ;
#8154 = DIRECTION ( 'NONE',  ( 1.000000000000000000, -0.000000000000000000, -1.450371633464475582E-15 ) ) ;
#8155 = EDGE_CURVE ( 'NONE', #9428, #4354, #17595, .T. ) ;
#8156 = DIRECTION ( 'NONE',  ( 0.000000000000000000, 1.000000000000000000, 0.000000000000000000 ) ) ;
#8157 = CARTESIAN_POINT ( 'NONE',  ( 0.000000000000000000, 23.00000000000000000, 0.000000000000000000 ) ) ;
#8158 = CARTESIAN_POINT ( 'NONE',  ( 4.549999999999999822, 0.000000000000000000, 0.000000000000000000 ) ) ;
#8159 = PLANE ( 'NONE',  #12619 ) ;
#8160 = FACE_OUTER_BOUND ( 'NONE', #7532, .T. ) ;
#8161 =( LENGTH_UNIT ( ) NAMED_UNIT ( * ) SI_UNIT ( .MILLI., .METRE. ) );
#8162 =( LENGTH_UNIT ( ) NAMED_UNIT ( * ) SI_UNIT ( .MILLI., .METRE. ) );
#8163 = CARTESIAN_POINT ( 'NONE',  ( 78.48937290013660117, 145.9162550801369491, 0.000000000000000000 ) ) ;
#8164 = EDGE_CURVE ( 'NONE', #17991, #4851, #11419, .T. ) ;
#8165 = DIRECTION ( 'NONE',  ( 1.000000000000000000, 9.815121534730718631E-17, -0.000000000000000000 ) ) ;
#8166 = MANIFOLD_SOLID_BREP ( 'Cut-Extrude7', #1063 ) ;
#8167 = EDGE_CURVE ( 'NONE', #19489, #5765, #19522, .T. ) ;
#8168 = VECTOR ( 'NONE', #1457, 1000.000000000000000 ) ;
#8169 = EDGE_CURVE ( 'NONE', #8090, #17153, #1691, .T. ) ;
#8170 = EDGE_LOOP ( 'NONE', ( #20007, #12572, #4875, #16651 ) ) ;
#8171 = AXIS2_PLACEMENT_3D ( 'NONE', #11520, #19530, #2435 ) ;
#8172 = CARTESIAN_POINT ( 'NONE',  ( -33.99999999999997158, 0.000000000000000000, 31.00000000000000000 ) ) ;
#8173 = ORIENTED_EDGE ( 'NONE', *, *, #9585, .T. ) ;
#8174 = CARTESIAN_POINT ( 'NONE',  ( 0.000000000000000000, 80.91625508013694912, 0.000000000000000000 ) ) ;
#8175 = EDGE_LOOP ( 'NONE', ( #7809, #6633, #10137, #17783 ) ) ;
#8176 = LINE ( 'NONE', #11245, #6766 ) ;
#8177 = DIRECTION ( 'NONE',  ( 1.000000000000000000, 0.000000000000000000, 0.000000000000000000 ) ) ;
#8178 = ORIENTED_EDGE ( 'NONE', *, *, #17702, .T. ) ;
#8179 = DIRECTION ( 'NONE',  ( -0.000000000000000000, -0.000000000000000000, 1.000000000000000000 ) ) ;
#8180 = LINE ( 'NONE', #11671, #12995 ) ;
#8181 = SURFACE_STYLE_FILL_AREA ( #9719 ) ;
#8182 = CARTESIAN_POINT ( 'NONE',  ( -1.000000000000009104, 141.3905724437643698, 484.7051316060566819 ) ) ;
#8183 = DIRECTION ( 'NONE',  ( -0.000000000000000000, 1.000000000000000000, -0.000000000000000000 ) ) ;
#8184 = LINE ( 'NONE', #16133, #2648 ) ;
#8185 = CARTESIAN_POINT ( 'NONE',  ( -37.00000000000000711, 10.00000000000000000, -23.00000000000000000 ) ) ;
#8186 = DIRECTION ( 'NONE',  ( 1.000000000000000000, 0.000000000000000000, 0.000000000000000000 ) ) ;
#8187 = VECTOR ( 'NONE', #16165, 1000.000000000000000 ) ;
#8188 = ORIENTED_EDGE ( 'NONE', *, *, #15822, .T. ) ;
#8189 = LINE ( 'NONE', #14363, #9556 ) ;
#8190 = CARTESIAN_POINT ( 'NONE',  ( 0.000000000000000000, 19.00100000000000122, 0.000000000000000000 ) ) ;
#8191 = ADVANCED_FACE ( 'NONE', ( #16574 ), #11825, .F. ) ;
#8192 = CARTESIAN_POINT ( 'NONE',  ( 133.4893729001365443, 103.1299228374914492, 220.6387154965113382 ) ) ;
#8193 = ORIENTED_EDGE ( 'NONE', *, *, #11019, .F. ) ;
#8194 = EDGE_LOOP ( 'NONE', ( #11866, #12506 ) ) ;
#8195 = ORIENTED_EDGE ( 'NONE', *, *, #19315, .T. ) ;
#8196 = EDGE_LOOP ( 'NONE', ( #3534, #11742, #10662, #7516 ) ) ;
#8197 = MANIFOLD_SOLID_BREP ( 'Cut-Extrude1', #6032 ) ;
#8198 = FACE_BOUND ( 'NONE', #18565, .T. ) ;
#8199 = AXIS2_PLACEMENT_3D ( 'NONE', #10757, #8814, #12014 ) ;
#8200 = VERTEX_POINT ( 'NONE', #16869 ) ;
#8201 =( LENGTH_UNIT ( ) NAMED_UNIT ( * ) SI_UNIT ( .MILLI., .METRE. ) );
#8202 = DIRECTION ( 'NONE',  ( -1.000000000000000000, 0.000000000000000000, 0.000000000000000000 ) ) ;
#8203 = CARTESIAN_POINT ( 'NONE',  ( 23.00000000000000711, 68.00000000000000000, -31.00000000000002487 ) ) ;
#8204 = CARTESIAN_POINT ( 'NONE',  ( 503.8334540492693918, 167.8734308960555950, 0.000000000000000000 ) ) ;
#8205 = FILL_AREA_STYLE ('',( #12958 ) ) ;
#8206 = CARTESIAN_POINT ( 'NONE',  ( 1.750000000000000000, -14.59999999999999964, -1.827785347727424768E-15 ) ) ;
#8207 = EDGE_LOOP ( 'NONE', ( #18031, #4403, #17947, #5200, #7304, #10663, #16680, #16654, #8724, #8377, #8568, #16468, #19950, #8804, #15373, #711, #9077, #13401, #17547, #5103, #14395, #13653, #17886, #15598, #3806, #12209, #15442, #9697 ) ) ;
#8208 = SURFACE_SIDE_STYLE ('',( #15751 ) ) ;
#8209 = CARTESIAN_POINT ( 'NONE',  ( 493.8117674897343363, 214.2156642432025251, 250.0000000000000000 ) ) ;
#8210 = DIRECTION ( 'NONE',  ( 1.000000000000000000, -0.000000000000000000, 0.000000000000000000 ) ) ;
#8211 = EDGE_CURVE ( 'NONE', #3208, #7486, #15327, .T. ) ;
#8212 = AXIS2_PLACEMENT_3D ( 'NONE', #13443, #7460, #19680 ) ;
#8213 = DIRECTION ( 'NONE',  ( 0.000000000000000000, 0.000000000000000000, 1.000000000000000000 ) ) ;
#8214 = CARTESIAN_POINT ( 'NONE',  ( -77.99033078109007988, 125.7247684487574304, 254.0000000000000000 ) ) ;
#8215 = ORIENTED_EDGE ( 'NONE', *, *, #15711, .T. ) ;
#8216 = ORIENTED_EDGE ( 'NONE', *, *, #7379, .F. ) ;
#8217 = ORIENTED_EDGE ( 'NONE', *, *, #2449, .T. ) ;
#8218 = CARTESIAN_POINT ( 'NONE',  ( 423.8334540492694487, 191.8198460455371333, 168.2339398819845826 ) ) ;
#8219 = CARTESIAN_POINT ( 'NONE',  ( -80.10586188290847076, 140.9786807048501487, 501.3714379820334557 ) ) ;
#8220 = CIRCLE ( 'NONE', #1252, 2.500000000000002220 ) ;
#8221 = ORIENTED_EDGE ( 'NONE', *, *, #10412, .T. ) ;
#8222 = CIRCLE ( 'NONE', #10182, 10.00000000000000888 ) ;
#8223 = CARTESIAN_POINT ( 'NONE',  ( 1.181929469893224560, 140.4048636633015406, 499.8237260975782874 ) ) ;
#8224 = AXIS2_PLACEMENT_3D ( 'NONE', #2397, #14997, #8704 ) ;
#8225 =( LENGTH_UNIT ( ) NAMED_UNIT ( * ) SI_UNIT ( .MILLI., .METRE. ) );
#8226 = ORIENTED_EDGE ( 'NONE', *, *, #14393, .T. ) ;
#8227 = EDGE_CURVE ( 'NONE', #7322, #8551, #2734, .T. ) ;
#8228 = CARTESIAN_POINT ( 'NONE',  ( 32.99999999999998579, 8.000000000000000000, 25.99999999999999645 ) ) ;
#8229 = LINE ( 'NONE', #6280, #13582 ) ;
#8230 = MANIFOLD_SOLID_BREP ( 'Fillet4', #2065 ) ;
#8231 = CARTESIAN_POINT ( 'NONE',  ( 78.48937290013660117, 103.1299228374914065, 79.58252780074349175 ) ) ;
#8232 = CARTESIAN_POINT ( 'NONE',  ( -23.00000000000002132, 10.00000000000000000, 37.00000000000000711 ) ) ;
#8233 = PLANE ( 'NONE',  #10135 ) ;
#8234 = DIRECTION ( 'NONE',  ( 1.000000000000000000, 0.000000000000000000, 0.000000000000000000 ) ) ;
#8235 = LINE ( 'NONE', #3803, #18830 ) ;
#8236 = CARTESIAN_POINT ( 'NONE',  ( -79.99999999999995737, 141.6406393683236331, 501.8237260975782874 ) ) ;
#8237 = LINE ( 'NONE', #6698, #14845 ) ;
#8238 = EDGE_LOOP ( 'NONE', ( #3982, #16785, #17404, #2672, #12376, #5624, #6818, #15676, #10460, #8215, #8276, #3942, #7094, #12024, #12136, #10745 ) ) ;
#8239 = VECTOR ( 'NONE', #6988, 1000.000000000000000 ) ;
#8240 = EDGE_CURVE ( 'NONE', #8829, #12714, #15114, .T. ) ;
#8241 = VECTOR ( 'NONE', #1544, 1000.000000000000000 ) ;
#8242 = ORIENTED_EDGE ( 'NONE', *, *, #11893, .F. ) ;
#8243 = VERTEX_POINT ( 'NONE', #16976 ) ;
#8244 = ADVANCED_FACE ( 'NONE', ( #4094 ), #15213, .F. ) ;
#8245 = LINE ( 'NONE', #11218, #11336 ) ;
#8246 = ORIENTED_EDGE ( 'NONE', *, *, #7465, .F. ) ;
#8247 = EDGE_LOOP ( 'NONE', ( #10609, #7866, #13856, #10400 ) ) ;
#8248 = DIRECTION ( 'NONE',  ( 0.000000000000000000, 1.000000000000000000, 0.000000000000000000 ) ) ;
#8249 = PRESENTATION_LAYER_ASSIGNMENT (  '', '', ( #9218 ) ) ;
#8250 = ADVANCED_FACE ( 'NONE', ( #1477 ), #3351, .F. ) ;
#8251 = DIRECTION ( 'NONE',  ( 0.000000000000000000, -0.000000000000000000, -1.000000000000000000 ) ) ;
#8252 = AXIS2_PLACEMENT_3D ( 'NONE', #11752, #16492, #13498 ) ;
#8253 = CYLINDRICAL_SURFACE ( 'NONE', #13282, 1.000000000000015987 ) ;
#8254 = DIRECTION ( 'NONE',  ( -1.000000000000000000, 0.000000000000000000, 0.000000000000000000 ) ) ;
#8255 = EDGE_CURVE ( 'NONE', #13965, #19767, #15572, .T. ) ;
#8256 = PRESENTATION_STYLE_ASSIGNMENT (( #5269 ) ) ;
#8257 = SURFACE_SIDE_STYLE ('',( #1944 ) ) ;
#8258 = MECHANICAL_DESIGN_GEOMETRIC_PRESENTATION_REPRESENTATION (  '', ( #11548 ), #14840 ) ;
#8259 = DIRECTION ( 'NONE',  ( 1.000000000000000000, -0.000000000000000000, -7.715811803773179210E-14 ) ) ;
#8260 = LINE ( 'NONE', #9806, #20219 ) ;
#8261 = MANIFOLD_SOLID_BREP ( 'Fillet1', #1387 ) ;
#8262 = EDGE_CURVE ( 'NONE', #16910, #2920, #10950, .T. ) ;
#8263 = AXIS2_PLACEMENT_3D ( 'NONE', #3138, #9418, #1557 ) ;
#8264 = AXIS2_PLACEMENT_3D ( 'NONE', #2055, #14854, #832 ) ;
#8265 = ORIENTED_EDGE ( 'NONE', *, *, #12142, .F. ) ;
#8266 = DIRECTION ( 'NONE',  ( 0.000000000000000000, 0.9187087263927379288, -0.3949357872488051813 ) ) ;
#8267 = UNCERTAINTY_MEASURE_WITH_UNIT (LENGTH_MEASURE( 1.000000000000000082E-05 ), #7302, 'distance_accuracy_value', 'NONE');
#8268 = ORIENTED_EDGE ( 'NONE', *, *, #1076, .F. ) ;
#8269 = ADVANCED_FACE ( 'NONE', ( #18902 ), #4497, .T. ) ;
#8270 =( NAMED_UNIT ( * ) PLANE_ANGLE_UNIT ( ) SI_UNIT ( $, .RADIAN. ) );
#8271 = VERTEX_POINT ( 'NONE', #17064 ) ;
#8272 = UNCERTAINTY_MEASURE_WITH_UNIT (LENGTH_MEASURE( 1.000000000000000082E-05 ), #16448, 'distance_accuracy_value', 'NONE');
#8273 = DIRECTION ( 'NONE',  ( 0.000000000000000000, 0.000000000000000000, -1.000000000000000000 ) ) ;
#8274 = LINE ( 'NONE', #17528, #19740 ) ;
#8275 = UNCERTAINTY_MEASURE_WITH_UNIT (LENGTH_MEASURE( 1.000000000000000082E-05 ), #17482, 'distance_accuracy_value', 'NONE');
#8276 = ORIENTED_EDGE ( 'NONE', *, *, #2580, .T. ) ;
#8277 = ADVANCED_FACE ( 'NONE', ( #18700 ), #17265, .F. ) ;
#8278 = DIRECTION ( 'NONE',  ( -0.000000000000000000, -0.000000000000000000, 1.000000000000000000 ) ) ;
#8279 = CARTESIAN_POINT ( 'NONE',  ( 4.286263797015737285E-15, -3.000000000000000000, -35.00000000000000711 ) ) ;
#8280 = LINE ( 'NONE', #10025, #17859 ) ;
#8281 = STYLED_ITEM ( 'NONE', ( #18005 ), #17398 ) ;
#8282 = SURFACE_STYLE_FILL_AREA ( #9412 ) ;
#8283 = CARTESIAN_POINT ( 'NONE',  ( 40.00000000000003553, 3.000000000000000000, -25.99999999999999645 ) ) ;
#8284 = FACE_OUTER_BOUND ( 'NONE', #14562, .T. ) ;
#8285 =( LENGTH_UNIT ( ) NAMED_UNIT ( * ) SI_UNIT ( .MILLI., .METRE. ) );
#8286 = VERTEX_POINT ( 'NONE', #2928 ) ;
#8287 = DIRECTION ( 'NONE',  ( -0.000000000000000000, -1.000000000000000000, -0.000000000000000000 ) ) ;
#8288 = ITEM_DEFINED_TRANSFORMATION ( 'NONE', 'NONE', #17551,  #2741 ) ;
#8289 = DIRECTION ( 'NONE',  ( 0.000000000000000000, 0.000000000000000000, 1.000000000000000000 ) ) ;
#8290 = ORIENTED_EDGE ( 'NONE', *, *, #6370, .T. ) ;
#8291 = EDGE_CURVE ( 'NONE', #19306, #4190, #14896, .T. ) ;
#8292 = ORIENTED_EDGE ( 'NONE', *, *, #2175, .F. ) ;
#8293 = ORIENTED_EDGE ( 'NONE', *, *, #11174, .F. ) ;
#8294 = AXIS2_PLACEMENT_3D ( 'NONE', #6265, #168, #4511 ) ;
#8295 = CARTESIAN_POINT ( 'NONE',  ( 40.00000000000001421, -3.000000000000000888, -150.0000000000000000 ) ) ;
#8296 =( NAMED_UNIT ( * ) SI_UNIT ( $, .STERADIAN. ) SOLID_ANGLE_UNIT ( ) );
#8297 = CIRCLE ( 'NONE', #10584, 3.883636366625808911 ) ;
#8298 = ORIENTED_EDGE ( 'NONE', *, *, #15928, .T. ) ;
#8299 = UNCERTAINTY_MEASURE_WITH_UNIT (LENGTH_MEASURE( 1.000000000000000082E-05 ), #6359, 'distance_accuracy_value', 'NONE');
#8300 = EDGE_CURVE ( 'NONE', #9381, #11894, #48, .T. ) ;
#8301 = FACE_OUTER_BOUND ( 'NONE', #19466, .T. ) ;
#8302 = CARTESIAN_POINT ( 'NONE',  ( -41.50085094405408626, 193.0431417881923153, 505.3921618609452935 ) ) ;
#8303 = ORIENTED_EDGE ( 'NONE', *, *, #1635, .F. ) ;
#8304 = FILL_AREA_STYLE ('',( #559 ) ) ;
#8305 = LINE ( 'NONE', #1985, #4040 ) ;
#8306 = DIRECTION ( 'NONE',  ( 0.000000000000000000, 0.000000000000000000, 1.000000000000000000 ) ) ;
#8307 = CARTESIAN_POINT ( 'NONE',  ( -211.5106270998635409, 123.1299228374912644, 170.4174721992565082 ) ) ;
#8308 = CARTESIAN_POINT ( 'NONE',  ( 0.000000000000000000, 216.7545334744432921, 495.1946179577816451 ) ) ;
#8309 = ORIENTED_EDGE ( 'NONE', *, *, #1277, .T. ) ;
#8310 = DIRECTION ( 'NONE',  ( 1.000000000000000000, 0.000000000000000000, -0.000000000000000000 ) ) ;
#8311 = CARTESIAN_POINT ( 'NONE',  ( -3.000000000000002220, 60.00000000000000711, 6.000000000000000000 ) ) ;
#8312 = SURFACE_SIDE_STYLE ('',( #17575 ) ) ;
#8313 = AXIS2_PLACEMENT_3D ( 'NONE', #15199, #10658, #12202 ) ;
#8314 =( NAMED_UNIT ( * ) SI_UNIT ( $, .STERADIAN. ) SOLID_ANGLE_UNIT ( ) );
#8315 = CARTESIAN_POINT ( 'NONE',  ( 93.50021617990246625, 59.20428337175810896, 9.743823552857557857 ) ) ;
#8316 = ORIENTED_EDGE ( 'NONE', *, *, #15822, .F. ) ;
#8317 = CARTESIAN_POINT ( 'NONE',  ( -1.387778780781445676E-14, 216.7545334744432921, 489.5655098179848892 ) ) ;
#8318 = CARTESIAN_POINT ( 'NONE',  ( 468.8334540492694487, 134.2156642432025251, 250.0000000000000000 ) ) ;
#8319 = ORIENTED_EDGE ( 'NONE', *, *, #12411, .F. ) ;
#8320 = COLOUR_RGB ( '', 0.09019608, 0.27058824, 0.51372549) ;
#8321 = ORIENTED_EDGE ( 'NONE', *, *, #8328, .F. ) ;
#8322 = ORIENTED_EDGE ( 'NONE', *, *, #9146, .T. ) ;
#8323 = DIRECTION ( 'NONE',  ( -0.000000000000000000, -1.000000000000000000, 0.000000000000000000 ) ) ;
#8324 = COLOUR_RGB ( '', 0.40784314, 0.44705882, 0.49803922) ;
#8325 = CARTESIAN_POINT ( 'NONE',  ( -79.91454752859293365, 140.3642491793935676, 501.8091283190183844 ) ) ;
#8326 = VERTEX_POINT ( 'NONE', #12432 ) ;
#8327 = CARTESIAN_POINT ( 'NONE',  ( 111.4893729001366012, 208.2227610943810134, 346.7612763259490407 ) ) ;
#8328 = EDGE_CURVE ( 'NONE', #15933, #9164, #10877, .T. ) ;
#8329 = CARTESIAN_POINT ( 'NONE',  ( -26.00000000000002842, 3.000000000000000000, -31.00000000000003197 ) ) ;
#8330 = AXIS2_PLACEMENT_3D ( 'NONE', #10980, #7883, #4808 ) ;
#8331 = VERTEX_POINT ( 'NONE', #6456 ) ;
#8332 = LINE ( 'NONE', #19338, #14479 ) ;
#8333 = CARTESIAN_POINT ( 'NONE',  ( 2.181929469893224560, 216.7545334744432921, 499.8237260975781169 ) ) ;
#8334 = DIRECTION ( 'NONE',  ( -0.000000000000000000, 1.000000000000000000, -0.000000000000000000 ) ) ;
#8335 = CARTESIAN_POINT ( 'NONE',  ( 53.48937290013659407, 129.7247684487574588, 370.0000000000000000 ) ) ;
#8336 =( NAMED_UNIT ( * ) PLANE_ANGLE_UNIT ( ) SI_UNIT ( $, .RADIAN. ) );
#8337 = CARTESIAN_POINT ( 'NONE',  ( -40.00000000000000000, 19.00000000000000000, -26.00000000000000355 ) ) ;
#8338 = LINE ( 'NONE', #19261, #17196 ) ;
#8339 = CARTESIAN_POINT ( 'NONE',  ( -20.99999999999999645, 8.000000000000000000, -35.00000000000000711 ) ) ;
#8340 = VERTEX_POINT ( 'NONE', #12745 ) ;
#8341 = DIRECTION ( 'NONE',  ( 0.000000000000000000, 0.000000000000000000, -1.000000000000000000 ) ) ;
#8342 = DIRECTION ( 'NONE',  ( 0.000000000000000000, -1.000000000000000000, 0.000000000000000000 ) ) ;
#8343 = AXIS2_PLACEMENT_3D ( 'NONE', #11094, #9446, #9339 ) ;
#8344 = VERTEX_POINT ( 'NONE', #651 ) ;
#8345 = TOROIDAL_SURFACE ( 'NONE', #2052, 8.000000000000000000, 1.000000000000000000 ) ;
#8346 = ORIENTED_EDGE ( 'NONE', *, *, #17121, .T. ) ;
#8347 = ORIENTED_EDGE ( 'NONE', *, *, #18438, .F. ) ;
#8348 = EDGE_LOOP ( 'NONE', ( #19970, #13632, #3853, #10464 ) ) ;
#8349 = VECTOR ( 'NONE', #12463, 1000.000000000000000 ) ;
#8350 = ORIENTED_EDGE ( 'NONE', *, *, #6131, .T. ) ;
#8351 = LINE ( 'NONE', #19352, #17316 ) ;
#8352 = SURFACE_SIDE_STYLE ('',( #6711 ) ) ;
#8353 = DIRECTION ( 'NONE',  ( 0.000000000000000000, 0.000000000000000000, -1.000000000000000000 ) ) ;
#8354 = AXIS2_PLACEMENT_3D ( 'NONE', #101, #3303, #10732 ) ;
#8355 = DIRECTION ( 'NONE',  ( 0.000000000000000000, 0.000000000000000000, -1.000000000000000000 ) ) ;
#8357 = ADVANCED_FACE ( 'NONE', ( #6665 ), #19314, .F. ) ;
#8356 = DIRECTION ( 'NONE',  ( 0.000000000000000000, 0.000000000000000000, -1.000000000000000000 ) ) ;
#8358 = CARTESIAN_POINT ( 'NONE',  ( 108.9893729001365870, 108.8727366810872468, 338.2196854716659118 ) ) ;
#8359 =( NAMED_UNIT ( * ) PLANE_ANGLE_UNIT ( ) SI_UNIT ( $, .RADIAN. ) );
#8360 = DIRECTION ( 'NONE',  ( -0.000000000000000000, -0.7071067811865455743, -0.7071067811865493491 ) ) ;
#8361 = MECHANICAL_DESIGN_GEOMETRIC_PRESENTATION_REPRESENTATION (  '', ( #4407 ), #10986 ) ;
#8362 = EDGE_CURVE ( 'NONE', #13442, #16217, #4356, .T. ) ;
#8363 = AXIS2_PLACEMENT_3D ( 'NONE', #1365, #15337, #4507 ) ;
#8364 =( NAMED_UNIT ( * ) PLANE_ANGLE_UNIT ( ) SI_UNIT ( $, .RADIAN. ) );
#8365 = DIRECTION ( 'NONE',  ( -1.000000000000000000, -0.000000000000000000, -0.000000000000000000 ) ) ;
#8366 = PRESENTATION_LAYER_ASSIGNMENT (  '', '', ( #15962 ) ) ;
#8367 = AXIS2_PLACEMENT_3D ( 'NONE', #9114, #7370, #4482 ) ;
#8368 = VECTOR ( 'NONE', #4474, 1000.000000000000000 ) ;
#8369 = VERTEX_POINT ( 'NONE', #6777 ) ;
#8370 = LINE ( 'NONE', #16418, #5120 ) ;
#8371 = ORIENTED_EDGE ( 'NONE', *, *, #6801, .T. ) ;
#8372 = EDGE_CURVE ( 'NONE', #6099, #14468, #9842, .T. ) ;
#8373 = FACE_OUTER_BOUND ( 'NONE', #998, .T. ) ;
#8374 = AXIS2_PLACEMENT_3D ( 'NONE', #2458, #16306, #6918 ) ;
#8375 = VERTEX_POINT ( 'NONE', #11588 ) ;
#8376 = CARTESIAN_POINT ( 'NONE',  ( 2.265596578422603396E-15, 8.000000000000000000, 18.50000000000000000 ) ) ;
#8377 = ORIENTED_EDGE ( 'NONE', *, *, #440, .T. ) ;
#8378 = CIRCLE ( 'NONE', #12646, 2.999999999999999112 ) ;
#8379 = FILL_AREA_STYLE ('',( #9919 ) ) ;
#8380 =( NAMED_UNIT ( * ) SI_UNIT ( $, .STERADIAN. ) SOLID_ANGLE_UNIT ( ) );
#8382 = EDGE_CURVE ( 'NONE', #14402, #13737, #8305, .T. ) ;
#8381 = CARTESIAN_POINT ( 'NONE',  ( 458.8334540492693350, 191.8198460455371333, 34.99421986894476788 ) ) ;
#8383 = STYLED_ITEM ( 'NONE', ( #2537 ), #12423 ) ;
#8384 = VECTOR ( 'NONE', #8165, 1000.000000000000000 ) ;
#8385 =( GEOMETRIC_REPRESENTATION_CONTEXT ( 3 ) GLOBAL_UNCERTAINTY_ASSIGNED_CONTEXT ( ( #6842 ) ) GLOBAL_UNIT_ASSIGNED_CONTEXT ( ( #11983, #8976, #1214 ) ) REPRESENTATION_CONTEXT ( 'NONE', 'WORKASPACE' ) );
#8386 =( NAMED_UNIT ( * ) SI_UNIT ( $, .STERADIAN. ) SOLID_ANGLE_UNIT ( ) );
#8387 = FACE_OUTER_BOUND ( 'NONE', #12569, .T. ) ;
#8388 = CARTESIAN_POINT ( 'NONE',  ( 111.4893729001366154, 49.66333933884488516, 252.0000000000000000 ) ) ;
#8389 = AXIS2_PLACEMENT_3D ( 'NONE', #3624, #13017, #6930 ) ;
#8390 = DIRECTION ( 'NONE',  ( 0.000000000000000000, 0.9980168174361081501, 0.06294785234384196737 ) ) ;
#8391 = ADVANCED_FACE ( 'NONE', ( #5416 ), #9745, .T. ) ;
#8392 = EDGE_LOOP ( 'NONE', ( #3025, #15104, #1859, #6350 ) ) ;
#8393 = DIRECTION ( 'NONE',  ( 0.000000000000000000, 0.000000000000000000, -1.000000000000000000 ) ) ;
#8394 = CARTESIAN_POINT ( 'NONE',  ( 20.99999999999996092, -20.00000000000000000, 35.00000000000000711 ) ) ;
#8395 =( NAMED_UNIT ( * ) SI_UNIT ( $, .STERADIAN. ) SOLID_ANGLE_UNIT ( ) );
#8396 = EDGE_CURVE ( 'NONE', #6404, #19010, #455, .T. ) ;
#8397 = STYLED_ITEM ( 'NONE', ( #11876 ), #1583 ) ;
#8398 = CIRCLE ( 'NONE', #5761, 10.00000000000000888 ) ;
#8399 = ORIENTED_EDGE ( 'NONE', *, *, #667, .F. ) ;
#8400 = EDGE_CURVE ( 'NONE', #417, #8375, #3564, .T. ) ;
#8401 = VERTEX_POINT ( 'NONE', #17975 ) ;
#8402 = ADVANCED_FACE ( 'NONE', ( #5007 ), #5216, .F. ) ;
#8403 = ORIENTED_EDGE ( 'NONE', *, *, #9922, .F. ) ;
#8404 = VECTOR ( 'NONE', #9667, 1000.000000000000000 ) ;
#8405 = FILL_AREA_STYLE ('',( #9938 ) ) ;
#8406 = CIRCLE ( 'NONE', #15317, 10.00000000000000888 ) ;
#8407 = ORIENTED_EDGE ( 'NONE', *, *, #17010, .F. ) ;
#8408 =( LENGTH_UNIT ( ) NAMED_UNIT ( * ) SI_UNIT ( .MILLI., .METRE. ) );
#8409 = LINE ( 'NONE', #2092, #8876 ) ;
#8410 = ORIENTED_EDGE ( 'NONE', *, *, #18313, .T. ) ;
#8411 = DIRECTION ( 'NONE',  ( 0.000000000000000000, 1.000000000000000000, 0.000000000000000000 ) ) ;
#8412 = AXIS2_PLACEMENT_3D ( 'NONE', #18237, #2252, #4149 ) ;
#8413 = DIRECTION ( 'NONE',  ( 0.000000000000000000, -1.000000000000000000, 0.000000000000000000 ) ) ;
#8414 = STYLED_ITEM ( 'NONE', ( #20340 ), #1151 ) ;
#8415 = AXIS2_PLACEMENT_3D ( 'NONE', #3383, #14608, #12773 ) ;
#8416 = FILL_AREA_STYLE_COLOUR ( '', #10628 ) ;
#8417 = DIRECTION ( 'NONE',  ( 0.000000000000000000, 1.000000000000000000, 0.000000000000000000 ) ) ;
#8418 = CARTESIAN_POINT ( 'NONE',  ( 5.945602903476760126, 0.000000000000000000, 0.000000000000000000 ) ) ;
#8419 = DIRECTION ( 'NONE',  ( 6.123031769111888756E-17, 0.000000000000000000, 1.000000000000000000 ) ) ;
#8420 = ORIENTED_EDGE ( 'NONE', *, *, #18532, .T. ) ;
#8421 = FILL_AREA_STYLE ('',( #862 ) ) ;
#8422 = FACE_OUTER_BOUND ( 'NONE', #13492, .T. ) ;
#8423 = AXIS2_PLACEMENT_3D ( 'NONE', #3131, #12412, #18678 ) ;
#8424 = LINE ( 'NONE', #12859, #14209 ) ;
#8425 = CARTESIAN_POINT ( 'NONE',  ( 31.00000000000003908, 19.00000000000000000, -26.00000000000000355 ) ) ;
#8426 = EDGE_CURVE ( 'NONE', #11681, #6976, #3723, .T. ) ;
#8427 = ORIENTED_EDGE ( 'NONE', *, *, #5505, .T. ) ;
#8428 = CIRCLE ( 'NONE', #8746, 10.00000000000000888 ) ;
#8429 = EDGE_CURVE ( 'NONE', #20152, #20212, #16059, .T. ) ;
#8430 = ORIENTED_EDGE ( 'NONE', *, *, #12654, .F. ) ;
#8431 = EDGE_CURVE ( 'NONE', #2341, #1465, #11392, .T. ) ;
#8432 = ORIENTED_EDGE ( 'NONE', *, *, #12033, .T. ) ;
#8433 = CYLINDRICAL_SURFACE ( 'NONE', #5002, 10.00000000000000888 ) ;
#8434 =( REPRESENTATION_RELATIONSHIP ('NONE','NONE', #12483, #4054 ) REPRESENTATION_RELATIONSHIP_WITH_TRANSFORMATION ( #1559 )SHAPE_REPRESENTATION_RELATIONSHIP( ) );
#8435 = DIRECTION ( 'NONE',  ( -0.000000000000000000, -1.000000000000000000, 0.000000000000000000 ) ) ;
#8436 = ORIENTED_EDGE ( 'NONE', *, *, #14342, .T. ) ;
#8437 = CARTESIAN_POINT ( 'NONE',  ( 1.181929469892950335, 147.7545334744432921, 496.6642397995874489 ) ) ;
#8438 = ORIENTED_EDGE ( 'NONE', *, *, #18614, .T. ) ;
#8439 = PLANE ( 'NONE',  #12848 ) ;
#8440 = CARTESIAN_POINT ( 'NONE',  ( 31.00000000000003908, 19.00000000000000000, -26.00000000000000355 ) ) ;
#8441 = CARTESIAN_POINT ( 'NONE',  ( 0.7345891654137221005, 139.7733146779539481, 489.5386252392920028 ) ) ;
#8442 = FILL_AREA_STYLE_COLOUR ( '', #6057 ) ;
#8443 = DIRECTION ( 'NONE',  ( 0.000000000000000000, 0.000000000000000000, -1.000000000000000000 ) ) ;
#8444 = CIRCLE ( 'NONE', #17962, 3.300000000000025135 ) ;
#8445 = CARTESIAN_POINT ( 'NONE',  ( 111.4893729001366012, 129.7247684487574588, 370.0000000000000000 ) ) ;
#8446 = LINE ( 'NONE', #9781, #719 ) ;
#8447 = CARTESIAN_POINT ( 'NONE',  ( 31.81980515339464333, 11.00000000000000000, 31.81980515339463622 ) ) ;
#8448 = SURFACE_STYLE_FILL_AREA ( #11526 ) ;
#8449 = VERTEX_POINT ( 'NONE', #17675 ) ;
#8450 = EDGE_CURVE ( 'NONE', #15201, #3980, #10623, .T. ) ;
#8451 = ORIENTED_EDGE ( 'NONE', *, *, #6231, .T. ) ;
#8452 = EDGE_LOOP ( 'NONE', ( #7321, #11723 ) ) ;
#8453 = PRESENTATION_LAYER_ASSIGNMENT (  '', '', ( #14036 ) ) ;
#8454 = ORIENTED_EDGE ( 'NONE', *, *, #19281, .T. ) ;
#8455 = ORIENTED_EDGE ( 'NONE', *, *, #4695, .F. ) ;
#8456 = CYLINDRICAL_SURFACE ( 'NONE', #16375, 3.300000000000011369 ) ;
#8457 = AXIS2_PLACEMENT_3D ( 'NONE', #8126, #14297, #19012 ) ;
#8458 = DIRECTION ( 'NONE',  ( 1.000000000000000000, -0.000000000000000000, 0.000000000000000000 ) ) ;
#8459 = FILL_AREA_STYLE ('',( #8646 ) ) ;
#8460 = DIRECTION ( 'NONE',  ( -0.000000000000000000, -0.000000000000000000, 1.000000000000000000 ) ) ;
#8461 = CARTESIAN_POINT ( 'NONE',  ( 111.4893729001365728, 210.4096692328539007, 345.9586017849864561 ) ) ;
#8462 = DIRECTION ( 'NONE',  ( -0.000000000000000000, -1.000000000000000000, -0.000000000000000000 ) ) ;
#8463 = CARTESIAN_POINT ( 'NONE',  ( 1.334572366541260990, 62.69404904380762389, 9.407584458684453921 ) ) ;
#8464 = DIRECTION ( 'NONE',  ( 0.000000000000000000, 0.000000000000000000, 1.000000000000000000 ) ) ;
#8465 = DIRECTION ( 'NONE',  ( -0.000000000000000000, -1.000000000000000000, -0.000000000000000000 ) ) ;
#8466 = VERTEX_POINT ( 'NONE', #8587 ) ;
#8467 = UNCERTAINTY_MEASURE_WITH_UNIT (LENGTH_MEASURE( 1.000000000000000082E-05 ), #15028, 'distance_accuracy_value', 'NONE');
#8468 = ORIENTED_EDGE ( 'NONE', *, *, #12073, .F. ) ;
#8469 = VERTEX_POINT ( 'NONE', #16661 ) ;
#8470 = AXIS2_PLACEMENT_3D ( 'NONE', #19160, #16111, #1938 ) ;
#8471 = DIRECTION ( 'NONE',  ( 0.000000000000000000, 0.000000000000000000, 1.000000000000000000 ) ) ;
#8472 = UNCERTAINTY_MEASURE_WITH_UNIT (LENGTH_MEASURE( 1.000000000000000082E-05 ), #10032, 'distance_accuracy_value', 'NONE');
#8473 = CARTESIAN_POINT ( 'NONE',  ( 82.88953019741013861, 80.91625508013694912, 245.0000000000000000 ) ) ;
#8474 = FACE_OUTER_BOUND ( 'NONE', #15185, .T. ) ;
#8475 = ORIENTED_EDGE ( 'NONE', *, *, #1563, .F. ) ;
#8476 = DIRECTION ( 'NONE',  ( -1.000000000000000000, -1.595148023886719315E-16, 0.000000000000000000 ) ) ;
#8477 = CARTESIAN_POINT ( 'NONE',  ( -78.99999999999995737, 152.4824555358010798, 510.3921618609452935 ) ) ;
#8478 = DIRECTION ( 'NONE',  ( 0.000000000000000000, -0.7071067811865753283, -0.7071067811865198172 ) ) ;
#8479 = ADVANCED_FACE ( 'NONE', ( #18158 ), #13276, .T. ) ;
#8480 =( NAMED_UNIT ( * ) SI_UNIT ( $, .STERADIAN. ) SOLID_ANGLE_UNIT ( ) );
#8481 = LINE ( 'NONE', #3851, #820 ) ;
#8482 = ORIENTED_EDGE ( 'NONE', *, *, #1534, .T. ) ;
#8483 = CARTESIAN_POINT ( 'NONE',  ( 34.00000000000002842, 0.000000000000000000, 23.00000000000000355 ) ) ;
#8484 = VECTOR ( 'NONE', #6589, 1000.000000000000000 ) ;
#8485 = EDGE_CURVE ( 'NONE', #10970, #11894, #18275, .T. ) ;
#8486 = VERTEX_POINT ( 'NONE', #11801 ) ;
#8487 = VERTEX_POINT ( 'NONE', #5604 ) ;
#8488 = DIRECTION ( 'NONE',  ( 2.135044278125300850E-16, -1.000000000000000000, 0.000000000000000000 ) ) ;
#8489 = EDGE_CURVE ( 'NONE', #3093, #825, #4063, .T. ) ;
#8490 = ORIENTED_EDGE ( 'NONE', *, *, #19952, .F. ) ;
#8491 = FILL_AREA_STYLE_COLOUR ( '', #16283 ) ;
#8492 = CARTESIAN_POINT ( 'NONE',  ( -23.00000000000002487, 10.00000000000000000, -36.99999999999999289 ) ) ;
#8493 = ORIENTED_EDGE ( 'NONE', *, *, #14047, .T. ) ;
#8494 = ADVANCED_FACE ( 'NONE', ( #19695 ), #13458, .F. ) ;
#8495 = CARTESIAN_POINT ( 'NONE',  ( 111.4893729001366012, 122.8810204491430369, 280.0825295754780768 ) ) ;
#8496 = SURFACE_STYLE_FILL_AREA ( #8304 ) ;
#8497 = DIRECTION ( 'NONE',  ( 0.000000000000000000, 0.000000000000000000, -1.000000000000000000 ) ) ;
#8498 = FACE_OUTER_BOUND ( 'NONE', #18838, .T. ) ;
#8499 = FACE_OUTER_BOUND ( 'NONE', #9290, .T. ) ;
#8500 = ORIENTED_EDGE ( 'NONE', *, *, #8372, .T. ) ;
#8501 = ADVANCED_FACE ( 'NONE', ( #11901 ), #746, .T. ) ;
#8502 = CARTESIAN_POINT ( 'NONE',  ( -1.734723475976807094E-15, 60.00000000000000711, 6.000000000000000000 ) ) ;
#8503 = CARTESIAN_POINT ( 'NONE',  ( -79.38892094406317312, 138.8697078648616525, 489.6181569159061837 ) ) ;
#8504 = FILL_AREA_STYLE ('',( #2105 ) ) ;
#8505 = ORIENTED_EDGE ( 'NONE', *, *, #8140, .T. ) ;
#8506 = DIRECTION ( 'NONE',  ( 0.000000000000000000, 0.000000000000000000, -1.000000000000000000 ) ) ;
#8507 = ORIENTED_EDGE ( 'NONE', *, *, #16115, .T. ) ;
#8508 = ADVANCED_FACE ( 'NONE', ( #4713 ), #9242, .F. ) ;
#8509 = ORIENTED_EDGE ( 'NONE', *, *, #2690, .F. ) ;
#8510 = ORIENTED_EDGE ( 'NONE', *, *, #18804, .F. ) ;
#8511 = EDGE_LOOP ( 'NONE', ( #5670, #8593, #11747, #10820 ) ) ;
#8512 = CARTESIAN_POINT ( 'NONE',  ( 31.00000000000000711, 68.00000000000000000, -30.99999999999999289 ) ) ;
#8513 = LINE ( 'NONE', #10371, #8133 ) ;
#8514 = VERTEX_POINT ( 'NONE', #18719 ) ;
#8515 = CARTESIAN_POINT ( 'NONE',  ( -23.00000000000002132, 10.00000000000000000, 31.00000000000003553 ) ) ;
#8516 = DIRECTION ( 'NONE',  ( -1.000000000000000000, -1.595148023886719315E-16, 0.000000000000000000 ) ) ;
#8517 = ORIENTED_EDGE ( 'NONE', *, *, #15801, .F. ) ;
#8518 = DIRECTION ( 'NONE',  ( 0.000000000000000000, 0.000000000000000000, -1.000000000000000000 ) ) ;
#8519 = DIRECTION ( 'NONE',  ( -0.000000000000000000, 1.000000000000000000, -0.000000000000000000 ) ) ;
#8520 = CARTESIAN_POINT ( 'NONE',  ( -34.99999999999998579, 0.000000000000000000, 23.50000000000000711 ) ) ;
#8521 = LINE ( 'NONE', #281, #2088 ) ;
#8522 = CARTESIAN_POINT ( 'NONE',  ( 2.204364238465236069E-16, 66.00000000000000000, -1.800000000000000711 ) ) ;
#8523 = CARTESIAN_POINT ( 'NONE',  ( 22.99999999999999289, 68.00000000000000000, 37.00000000000002132 ) ) ;
#8524 = CARTESIAN_POINT ( 'NONE',  ( 3.000000000000000000, 6.000000000000000000, 22.00000000000000000 ) ) ;
#8525 = CARTESIAN_POINT ( 'NONE',  ( 21.99999999999998224, 8.000000000000000000, -32.99999999999999289 ) ) ;
#8526 = UNCERTAINTY_MEASURE_WITH_UNIT (LENGTH_MEASURE( 1.000000000000000082E-05 ), #1369, 'distance_accuracy_value', 'NONE');
#8527 = CARTESIAN_POINT ( 'NONE',  ( 0.000000000000000000, 23.00000000000000000, 0.000000000000000000 ) ) ;
#8528 = SURFACE_STYLE_USAGE ( .BOTH. , #16395 ) ;
#8529 = EDGE_LOOP ( 'NONE', ( #9855, #6505, #8753, #8430, #3907 ) ) ;
#8530 = VERTEX_POINT ( 'NONE', #11101 ) ;
#8531 = PRESENTATION_LAYER_ASSIGNMENT (  '', '', ( #4258 ) ) ;
#8532 = COLOUR_RGB ( '', 0.31764706, 0.68627451, 0.89019608) ;
#8533 = EDGE_LOOP ( 'NONE', ( #11582, #11150, #16723, #17556, #11710, #4216, #19447, #18430, #9886, #4221 ) ) ;
#8534 = STYLED_ITEM ( 'NONE', ( #18621 ), #5523 ) ;
#8536 = ORIENTED_EDGE ( 'NONE', *, *, #13554, .T. ) ;
#8535 = EDGE_CURVE ( 'NONE', #17405, #19090, #11581, .T. ) ;
#8537 = ORIENTED_EDGE ( 'NONE', *, *, #13284, .T. ) ;
#8538 = CARTESIAN_POINT ( 'NONE',  ( 463.8334540492693350, 191.8198460455371333, 24.99421986894476078 ) ) ;
#8539 = DIRECTION ( 'NONE',  ( 1.000000000000000000, -0.000000000000000000, 0.000000000000000000 ) ) ;
#8540 = SURFACE_STYLE_USAGE ( .BOTH. , #5360 ) ;
#8541 = DIRECTION ( 'NONE',  ( 0.000000000000000000, 0.000000000000000000, -1.000000000000000000 ) ) ;
#8542 = FACE_OUTER_BOUND ( 'NONE', #6795, .T. ) ;
#8543 = AXIS2_PLACEMENT_3D ( 'NONE', #19734, #12052, #13689 ) ;
#8544 = CARTESIAN_POINT ( 'NONE',  ( 109.4893729001366012, 127.7247684487574588, 368.0000000000000000 ) ) ;
#8545 = COLOUR_RGB ( '', 0.40784314, 0.44705882, 0.49803922) ;
#8546 = LINE ( 'NONE', #14434, #2321 ) ;
#8547 = AXIS2_PLACEMENT_3D ( 'NONE', #10235, #2602, #4177 ) ;
#8548 = SURFACE_STYLE_FILL_AREA ( #11762 ) ;
#8549 = DIRECTION ( 'NONE',  ( -0.000000000000000000, -1.000000000000000000, -0.000000000000000000 ) ) ;
#8550 = EDGE_LOOP ( 'NONE', ( #9125, #3265, #2758, #18101 ) ) ;
#8551 = VERTEX_POINT ( 'NONE', #2953 ) ;
#8552 = DIRECTION ( 'NONE',  ( -1.000000000000000000, 0.000000000000000000, -1.156482317317870344E-15 ) ) ;
#8553 = ORIENTED_EDGE ( 'NONE', *, *, #11511, .T. ) ;
#8554 = VERTEX_POINT ( 'NONE', #4614 ) ;
#8555 = CIRCLE ( 'NONE', #18424, 4.999999999999997335 ) ;
#8556 = CIRCLE ( 'NONE', #6613, 9.999999999999998224 ) ;
#8557 = AXIS2_PLACEMENT_3D ( 'NONE', #18153, #7258, #8803 ) ;
#8558 = CARTESIAN_POINT ( 'NONE',  ( 0.000000000000000000, 3.000000000000000000, 0.000000000000000000 ) ) ;
#8559 = CARTESIAN_POINT ( 'NONE',  ( 153.4893729001366864, 123.1299228374914634, 170.4174721992565082 ) ) ;
#8560 = EDGE_LOOP ( 'NONE', ( #7165, #5452, #7415, #2724 ) ) ;
#8561 = CARTESIAN_POINT ( 'NONE',  ( 25.99999999999999645, 68.00000000000000000, -39.99999999999999289 ) ) ;
#8562 = ADVANCED_FACE ( 'NONE', ( #20360 ), #10902, .F. ) ;
#8563 = DIRECTION ( 'NONE',  ( 0.000000000000000000, -0.7071067811865336949, -0.7071067811865614505 ) ) ;
#8564 = CARTESIAN_POINT ( 'NONE',  ( -211.5106270998635409, 113.1299228374912502, 170.4174721992565082 ) ) ;
#8565 = DIRECTION ( 'NONE',  ( 0.000000000000000000, 0.000000000000000000, 1.000000000000000000 ) ) ;
#8566 = CARTESIAN_POINT ( 'NONE',  ( 31.81980515339464333, 8.000000000000000000, -28.51980515339463906 ) ) ;
#8567 = FACE_OUTER_BOUND ( 'NONE', #15884, .T. ) ;
#8568 = ORIENTED_EDGE ( 'NONE', *, *, #19079, .T. ) ;
#8569 = FACE_BOUND ( 'NONE', #9050, .T. ) ;
#8570 = LINE ( 'NONE', #19681, #19534 ) ;
#8571 =( LENGTH_UNIT ( ) NAMED_UNIT ( * ) SI_UNIT ( .MILLI., .METRE. ) );
#8572 = VECTOR ( 'NONE', #1769, 1000.000000000000000 ) ;
#8573 = VECTOR ( 'NONE', #14237, 1000.000000000000000 ) ;
#8574 = CIRCLE ( 'NONE', #19420, 10.00000000000000888 ) ;
#8575 = CARTESIAN_POINT ( 'NONE',  ( -21.85283368562565443, 319.7545334744432353, 485.1700099148404774 ) ) ;
#8576 = AXIS2_PLACEMENT_3D ( 'NONE', #18330, #2666, #5662 ) ;
#8577 = VERTEX_POINT ( 'NONE', #4827 ) ;
#8578 = EDGE_CURVE ( 'NONE', #10797, #4918, #7950, .T. ) ;
#8579 = ORIENTED_EDGE ( 'NONE', *, *, #10249, .T. ) ;
#8580 = VERTEX_POINT ( 'NONE', #6473 ) ;
#8581 = FACE_BOUND ( 'NONE', #15305, .T. ) ;
#8582 = MECHANICAL_DESIGN_GEOMETRIC_PRESENTATION_REPRESENTATION (  '', ( #8281 ), #17814 ) ;
#8583 = DIRECTION ( 'NONE',  ( 0.000000000000000000, 0.000000000000000000, -1.000000000000000000 ) ) ;
#8584 = ORIENTED_EDGE ( 'NONE', *, *, #12055, .F. ) ;
#8585 = LINE ( 'NONE', #744, #5579 ) ;
#8586 = CARTESIAN_POINT ( 'NONE',  ( 178.4893729001365443, 145.9162550801369491, 0.000000000000000000 ) ) ;
#8587 = CARTESIAN_POINT ( 'NONE',  ( 35.00000000000000711, 19.00000000000000000, 20.99999999999999289 ) ) ;
#8588 = UNCERTAINTY_MEASURE_WITH_UNIT (LENGTH_MEASURE( 1.000000000000000082E-05 ), #3762, 'distance_accuracy_value', 'NONE');
#8589 = CARTESIAN_POINT ( 'NONE',  ( 36.99999999999999289, 10.00000000000000000, -22.99999999999999645 ) ) ;
#8590 = FILL_AREA_STYLE ('',( #16363 ) ) ;
#8591 = EDGE_CURVE ( 'NONE', #18058, #506, #8297, .T. ) ;
#8592 = CARTESIAN_POINT ( 'NONE',  ( -39.99999999999997868, 0.000000000000000000, 26.00000000000000355 ) ) ;
#8593 = ORIENTED_EDGE ( 'NONE', *, *, #13554, .F. ) ;
#8594 = CARTESIAN_POINT ( 'NONE',  ( 458.8334540492693350, 191.8198460455371333, 24.99421986894476078 ) ) ;
#8595 = FACE_OUTER_BOUND ( 'NONE', #1181, .T. ) ;
#8596 = LINE ( 'NONE', #16551, #4965 ) ;
#8597 = PLANE ( 'NONE',  #5709 ) ;
#8598 = DIRECTION ( 'NONE',  ( 1.000000000000000000, 0.000000000000000000, 0.000000000000000000 ) ) ;
#8599 = EDGE_LOOP ( 'NONE', ( #9169, #6069, #17663, #10657 ) ) ;
#8600 = EDGE_CURVE ( 'NONE', #11049, #15475, #14199, .T. ) ;
#8601 = CARTESIAN_POINT ( 'NONE',  ( -78.99999999999995737, 146.1184945051222428, 479.9772095446988374 ) ) ;
#8602 = ORIENTED_EDGE ( 'NONE', *, *, #8954, .F. ) ;
#8603 = PRESENTATION_LAYER_ASSIGNMENT (  '', '', ( #10253 ) ) ;
#8604 = ORIENTED_EDGE ( 'NONE', *, *, #17597, .F. ) ;
#8605 =( GEOMETRIC_REPRESENTATION_CONTEXT ( 3 ) GLOBAL_UNCERTAINTY_ASSIGNED_CONTEXT ( ( #3400 ) ) GLOBAL_UNIT_ASSIGNED_CONTEXT ( ( #11505, #9859, #16274 ) ) REPRESENTATION_CONTEXT ( 'NONE', 'WORKASPACE' ) );
#8606 = ORIENTED_EDGE ( 'NONE', *, *, #19373, .T. ) ;
#8607 = ADVANCED_FACE ( 'NONE', ( #17287 ), #6372, .F. ) ;
#8608 = ORIENTED_EDGE ( 'NONE', *, *, #4294, .F. ) ;
#8609 = ORIENTED_EDGE ( 'NONE', *, *, #19901, .T. ) ;
#8610 = CARTESIAN_POINT ( 'NONE',  ( 30.99999999999997868, 0.000000000000000000, -30.99999999999999645 ) ) ;
#8611 = ADVANCED_FACE ( 'NONE', ( #6066 ), #17477, .F. ) ;
#8612 = DIRECTION ( 'NONE',  ( -0.000000000000000000, -1.000000000000000000, -0.000000000000000000 ) ) ;
#8613 = EDGE_LOOP ( 'NONE', ( #3375, #10637, #12690, #19620 ) ) ;
#8614 = FILL_AREA_STYLE_COLOUR ( '', #19882 ) ;
#8615 = SURFACE_SIDE_STYLE ('',( #19426 ) ) ;
#8616 = CARTESIAN_POINT ( 'NONE',  ( 1.347066989204613998E-15, 0.000000000000000000, 22.00000000000000000 ) ) ;
#8617 = AXIS2_PLACEMENT_3D ( 'NONE', #5204, #16241, #15931 ) ;
#8618 = CARTESIAN_POINT ( 'NONE',  ( -22.99999999999999645, 68.00000000000000000, 37.00000000000002132 ) ) ;
#8619 = CARTESIAN_POINT ( 'NONE',  ( -0.03866188257987528132, 139.1517308181911403, 488.4190873714470058 ) ) ;
#8620 = EDGE_CURVE ( 'NONE', #14600, #8326, #9584, .T. ) ;
#8621 = CARTESIAN_POINT ( 'NONE',  ( 463.8334540492693350, 214.2156642432025251, 0.000000000000000000 ) ) ;
#8622 =( GEOMETRIC_REPRESENTATION_CONTEXT ( 3 ) GLOBAL_UNCERTAINTY_ASSIGNED_CONTEXT ( ( #9790 ) ) GLOBAL_UNIT_ASSIGNED_CONTEXT ( ( #12118, #5534, #8920 ) ) REPRESENTATION_CONTEXT ( 'NONE', 'WORKASPACE' ) );
#8623 = DIRECTION ( 'NONE',  ( -1.000000000000000000, 0.000000000000000000, -0.000000000000000000 ) ) ;
#8624 = DIRECTION ( 'NONE',  ( 1.000000000000000000, 0.000000000000000000, 0.000000000000000000 ) ) ;
#8625 = LINE ( 'NONE', #7106, #7670 ) ;
#8626 =( LENGTH_UNIT ( ) NAMED_UNIT ( * ) SI_UNIT ( .MILLI., .METRE. ) );
#8627 = VECTOR ( 'NONE', #13570, 1000.000000000000000 ) ;
#8628 = CARTESIAN_POINT ( 'NONE',  ( 153.4893729001366864, 123.1299228374914634, 220.6387154965113382 ) ) ;
#8629 = CARTESIAN_POINT ( 'NONE',  ( 20.99999999999996092, 0.000000000000000000, 32.50000000000000711 ) ) ;
#8630 = ORIENTED_EDGE ( 'NONE', *, *, #4486, .T. ) ;
#8631 = EDGE_CURVE ( 'NONE', #4888, #15103, #14396, .T. ) ;
#8632 = AXIS2_PLACEMENT_3D ( 'NONE', #16453, #2301, #16368 ) ;
#8633 = VERTEX_POINT ( 'NONE', #5233 ) ;
#8634 = CIRCLE ( 'NONE', #9962, 3.283624802691453848 ) ;
#8635 = COLOUR_RGB ( '', 0.31764706, 0.68627451, 0.89019608) ;
#8636 = PRODUCT_DEFINITION_CONTEXT ( 'detailed design', #11975, 'design' ) ;
#8637 = ADVANCED_FACE ( 'NONE', ( #5029 ), #19517, .F. ) ;
#8638 = EDGE_LOOP ( 'NONE', ( #8217, #4436, #5929, #2568 ) ) ;
#8639 = AXIS2_PLACEMENT_3D ( 'NONE', #11704, #1886, #14576 ) ;
#8640 = ORIENTED_EDGE ( 'NONE', *, *, #1901, .F. ) ;
#8641 = ORIENTED_EDGE ( 'NONE', *, *, #4078, .F. ) ;
#8642 = DIRECTION ( 'NONE',  ( 1.000000000000000000, 1.197852309262419498E-15, -0.000000000000000000 ) ) ;
#8643 = DIRECTION ( 'NONE',  ( 0.000000000000000000, -0.000000000000000000, 1.000000000000000000 ) ) ;
#8644 = LINE ( 'NONE', #14733, #2294 ) ;
#8645 = VECTOR ( 'NONE', #19216, 1000.000000000000000 ) ;
#8646 = FILL_AREA_STYLE_COLOUR ( '', #7703 ) ;
#8647 = STYLED_ITEM ( 'NONE', ( #2178 ), #11440 ) ;
#8648 = CARTESIAN_POINT ( 'NONE',  ( 458.8334540492693350, 242.8734308960556234, 250.0000000000000000 ) ) ;
#8649 = DIRECTION ( 'NONE',  ( -1.000000000000000000, -0.000000000000000000, 1.156482317317883755E-15 ) ) ;
#8650 = FILL_AREA_STYLE ('',( #2240 ) ) ;
#8651 = DIRECTION ( 'NONE',  ( -0.000000000000000000, -1.000000000000000000, -0.000000000000000000 ) ) ;
#8652 = FILL_AREA_STYLE_COLOUR ( '', #5727 ) ;
#8653 = DIRECTION ( 'NONE',  ( 1.000000000000000000, 0.000000000000000000, 0.000000000000000000 ) ) ;
#8654 = CIRCLE ( 'NONE', #3719, 2.500000000000002220 ) ;
#8655 = VECTOR ( 'NONE', #5750, 1000.000000000000000 ) ;
#8656 = CARTESIAN_POINT ( 'NONE',  ( 0.000000000000000000, 140.4048636633015406, 499.8237260975782874 ) ) ;
#8657 = EDGE_CURVE ( 'NONE', #6561, #13659, #16381, .T. ) ;
#8658 = CARTESIAN_POINT ( 'NONE',  ( 463.8334540492693918, 167.8734308960555950, 0.000000000000000000 ) ) ;
#8659 = CARTESIAN_POINT ( 'NONE',  ( -19.00000000000001776, 10.00000000000000000, 40.00000000000000711 ) ) ;
#8660 = CLOSED_SHELL ( 'NONE', ( #3379, #2791, #14429, #13055, #4942, #15934, #9121, #58, #13668, #7531, #3699, #5731, #14038, #13406, #13947, #18026, #1877, #7191, #2576, #14544, #4592, #3247, #19920, #7334, #20311, #11046, #8985, #2534, #19996, #19327, #2446, #2600, #705 ) ) ;
#8661 = EDGE_CURVE ( 'NONE', #7678, #16895, #14212, .T. ) ;
#8662 = ORIENTED_EDGE ( 'NONE', *, *, #13419, .T. ) ;
#8663 = ORIENTED_EDGE ( 'NONE', *, *, #2961, .T. ) ;
#8664 = DIRECTION ( 'NONE',  ( 1.000000000000000000, -0.000000000000000000, 0.000000000000000000 ) ) ;
#8665 = UNCERTAINTY_MEASURE_WITH_UNIT (LENGTH_MEASURE( 1.000000000000000082E-05 ), #5784, 'distance_accuracy_value', 'NONE');
#8666 = ORIENTED_EDGE ( 'NONE', *, *, #11842, .F. ) ;
#8667 = ORIENTED_EDGE ( 'NONE', *, *, #14645, .T. ) ;
#8668 = STYLED_ITEM ( 'NONE', ( #9277 ), #14002 ) ;
#8669 = VECTOR ( 'NONE', #19113, 1000.000000000000000 ) ;
#8670 = ADVANCED_FACE ( 'NONE', ( #1903 ), #8433, .F. ) ;
#8671 = VERTEX_POINT ( 'NONE', #579 ) ;
#8672 = DIRECTION ( 'NONE',  ( 0.000000000000000000, -1.000000000000000000, 0.000000000000000000 ) ) ;
#8673 = UNCERTAINTY_MEASURE_WITH_UNIT (LENGTH_MEASURE( 1.000000000000000082E-05 ), #2988, 'distance_accuracy_value', 'NONE');
#8674 =( LENGTH_UNIT ( ) NAMED_UNIT ( * ) SI_UNIT ( .MILLI., .METRE. ) );
#8675 = ORIENTED_EDGE ( 'NONE', *, *, #1455, .F. ) ;
#8676 = DIRECTION ( 'NONE',  ( 1.000000000000000000, -0.000000000000000000, -0.000000000000000000 ) ) ;
#8677 = CARTESIAN_POINT ( 'NONE',  ( -79.99999999999995737, 216.7545334744432921, 495.1946179577816451 ) ) ;
#8678 = LINE ( 'NONE', #12085, #16888 ) ;
#8679 = AXIS2_PLACEMENT_3D ( 'NONE', #14701, #1996, #571 ) ;
#8680 = DIRECTION ( 'NONE',  ( 0.000000000000000000, 0.000000000000000000, 1.000000000000000000 ) ) ;
#8681 =( LENGTH_UNIT ( ) NAMED_UNIT ( * ) SI_UNIT ( .MILLI., .METRE. ) );
#8682 = DIRECTION ( 'NONE',  ( 1.000000000000000000, 0.000000000000000000, 0.000000000000000000 ) ) ;
#8683 = EDGE_LOOP ( 'NONE', ( #16003, #16464, #201, #7927 ) ) ;
#8684 =( NAMED_UNIT ( * ) SI_UNIT ( $, .STERADIAN. ) SOLID_ANGLE_UNIT ( ) );
#8685 = VECTOR ( 'NONE', #18822, 1000.000000000000000 ) ;
#8686 = MECHANICAL_DESIGN_GEOMETRIC_PRESENTATION_REPRESENTATION (  '', ( #19531 ), #7063 ) ;
#8687 = CARTESIAN_POINT ( 'NONE',  ( 35.99999999999999289, 10.00000000000000000, 17.99999999999998934 ) ) ;
#8688 = PRESENTATION_LAYER_ASSIGNMENT (  '', '', ( #9668 ) ) ;
#8689 = AXIS2_PLACEMENT_3D ( 'NONE', #10132, #16347, #6951 ) ;
#8690 = DIRECTION ( 'NONE',  ( 0.000000000000000000, 1.000000000000000000, 0.000000000000000000 ) ) ;
#8691 = MECHANICAL_DESIGN_GEOMETRIC_PRESENTATION_REPRESENTATION (  '', ( #3425 ), #1423 ) ;
#8692 = EDGE_CURVE ( 'NONE', #715, #6680, #6889, .T. ) ;
#8693 = VECTOR ( 'NONE', #9685, 1000.000000000000000 ) ;
#8694 = ORIENTED_EDGE ( 'NONE', *, *, #18049, .F. ) ;
#8695 = ORIENTED_EDGE ( 'NONE', *, *, #5253, .F. ) ;
#8696 = ORIENTED_EDGE ( 'NONE', *, *, #13338, .T. ) ;
#8697 = STYLED_ITEM ( 'NONE', ( #10678 ), #12465 ) ;
#8698 = CARTESIAN_POINT ( 'NONE',  ( 9.796850830579020038E-16, 6.000000000000000000, 22.00000000000000000 ) ) ;
#8699 = VECTOR ( 'NONE', #8365, 1000.000000000000000 ) ;
#8700 = FACE_BOUND ( 'NONE', #16254, .T. ) ;
#8701 = UNCERTAINTY_MEASURE_WITH_UNIT (LENGTH_MEASURE( 1.000000000000000082E-05 ), #6096, 'distance_accuracy_value', 'NONE');
#8702 = STYLED_ITEM ( 'NONE', ( #5823 ), #15140 ) ;
#8703 = ORIENTED_EDGE ( 'NONE', *, *, #187, .F. ) ;
#8704 = DIRECTION ( 'NONE',  ( 0.000000000000000000, 0.000000000000000000, 1.000000000000000000 ) ) ;
#8705 = CARTESIAN_POINT ( 'NONE',  ( -79.99999999999995737, 147.7545334744432921, 491.0690926367356042 ) ) ;
#8706 = VECTOR ( 'NONE', #10036, 1000.000000000000000 ) ;
#8707 = CARTESIAN_POINT ( 'NONE',  ( -22.00000000000001776, 10.00000000000000000, 33.00000000000000711 ) ) ;
#8708 = FACE_OUTER_BOUND ( 'NONE', #11634, .T. ) ;
#8709 = FILL_AREA_STYLE ('',( #19609 ) ) ;
#8710 = PRESENTATION_LAYER_ASSIGNMENT (  '', '', ( #15975 ) ) ;
#8711 = FACE_OUTER_BOUND ( 'NONE', #17581, .T. ) ;
#8712 = STYLED_ITEM ( 'NONE', ( #1702 ), #808 ) ;
#8713 = VERTEX_POINT ( 'NONE', #5331 ) ;
#8714 = FACE_OUTER_BOUND ( 'NONE', #365, .T. ) ;
#8715 = DIRECTION ( 'NONE',  ( 0.000000000000000000, 0.000000000000000000, -1.000000000000000000 ) ) ;
#8716 = FACE_OUTER_BOUND ( 'NONE', #4578, .T. ) ;
#8717 = VECTOR ( 'NONE', #19793, 1000.000000000000000 ) ;
#8718 = ADVANCED_FACE ( 'NONE', ( #11607 ), #10071, .T. ) ;
#8719 =( LENGTH_UNIT ( ) NAMED_UNIT ( * ) SI_UNIT ( .MILLI., .METRE. ) );
#8720 = AXIS2_PLACEMENT_3D ( 'NONE', #1766, #6535, #12823 ) ;
#8721 = ORIENTED_EDGE ( 'NONE', *, *, #6504, .F. ) ;
#8722 = VECTOR ( 'NONE', #15798, 1000.000000000000000 ) ;
#8723 = STYLED_ITEM ( 'NONE', ( #5043 ), #15275 ) ;
#8724 = ORIENTED_EDGE ( 'NONE', *, *, #10742, .F. ) ;
#8725 = COLOUR_RGB ( '', 0.08235294, 0.09019608, 0.10196078) ;
#8726 = ORIENTED_EDGE ( 'NONE', *, *, #7152, .T. ) ;
#8727 = EDGE_CURVE ( 'NONE', #19572, #8200, #15205, .T. ) ;
#8728 = VECTOR ( 'NONE', #6964, 1000.000000000000000 ) ;
#8729 = EDGE_LOOP ( 'NONE', ( #9787, #10748, #4671 ) ) ;
#8730 = CARTESIAN_POINT ( 'NONE',  ( 0.000000000000000000, 10.00000000000000000, 0.000000000000000000 ) ) ;
#8731 = DIRECTION ( 'NONE',  ( 0.000000000000000000, 0.000000000000000000, -1.000000000000000000 ) ) ;
#8732 = ORIENTED_EDGE ( 'NONE', *, *, #12783, .F. ) ;
#8733 = PRODUCT_RELATED_PRODUCT_CATEGORY ( 'part', '', ( #3169 ) ) ;
#8734 = CIRCLE ( 'NONE', #16004, 3.000000000000002665 ) ;
#8735 = FACE_OUTER_BOUND ( 'NONE', #17174, .T. ) ;
#8736 = VECTOR ( 'NONE', #16478, 1000.000000000000000 ) ;
#8737 = CARTESIAN_POINT ( 'NONE',  ( 0.000000000000000000, 3.000000000000000888, 0.000000000000000000 ) ) ;
#8738 = CARTESIAN_POINT ( 'NONE',  ( 0.4691783309273026004, 138.7756623317111462, 490.4420716635970052 ) ) ;
#8739 = CARTESIAN_POINT ( 'NONE',  ( 53.48937290013659407, 145.9162550801369491, 250.0000000000000000 ) ) ;
#8740 = CARTESIAN_POINT ( 'NONE',  ( 1.163414459189985485E-15, 66.00000000000000000, 9.500000000000000000 ) ) ;
#8741 = EDGE_CURVE ( 'NONE', #9449, #19389, #18568, .T. ) ;
#8742 = SURFACE_SIDE_STYLE ('',( #16878 ) ) ;
#8743 = DIRECTION ( 'NONE',  ( -1.000000000000000000, 0.000000000000000000, -0.000000000000000000 ) ) ;
#8744 = CARTESIAN_POINT ( 'NONE',  ( 30.99999999999999645, 68.00000000000000000, 31.00000000000001066 ) ) ;
#8745 = DIRECTION ( 'NONE',  ( -1.000000000000000000, 0.000000000000000000, 0.000000000000000000 ) ) ;
#8746 = AXIS2_PLACEMENT_3D ( 'NONE', #10643, #4565, #15720 ) ;
#8747 = DIRECTION ( 'NONE',  ( -1.445602896647339163E-16, 1.000000000000000000, 0.000000000000000000 ) ) ;
#8748 = SURFACE_STYLE_FILL_AREA ( #15342 ) ;
#8749 = FILL_AREA_STYLE ('',( #8843 ) ) ;
#8750 = EDGE_CURVE ( 'NONE', #593, #19577, #16466, .T. ) ;
#8751 = ORIENTED_EDGE ( 'NONE', *, *, #1044, .F. ) ;
#8752 = AXIS2_PLACEMENT_3D ( 'NONE', #9215, #8825, #8916 ) ;
#8753 = ORIENTED_EDGE ( 'NONE', *, *, #17010, .T. ) ;
#8754 = ADVANCED_FACE ( 'NONE', ( #7091, #10161 ), #13384, .T. ) ;
#8755 = ORIENTED_EDGE ( 'NONE', *, *, #8155, .T. ) ;
#8756 = EDGE_CURVE ( 'NONE', #12453, #17418, #11821, .T. ) ;
#8757 = ORIENTED_EDGE ( 'NONE', *, *, #11779, .F. ) ;
#8758 = SURFACE_STYLE_FILL_AREA ( #2456 ) ;
#8759 = AXIS2_PLACEMENT_3D ( 'NONE', #17106, #2986, #9275 ) ;
#8760 = CARTESIAN_POINT ( 'NONE',  ( 0.000000000000000000, 145.9162550801369491, 250.0000000000000000 ) ) ;
#8761 = DIRECTION ( 'NONE',  ( -1.000000000000000000, -0.000000000000000000, -0.000000000000000000 ) ) ;
#8762 = ADVANCED_FACE ( 'NONE', ( #1323 ), #15606, .F. ) ;
#8763 = DIRECTION ( 'NONE',  ( -1.000000000000000000, -0.000000000000000000, -0.000000000000000000 ) ) ;
#8764 = VECTOR ( 'NONE', #6656, 1000.000000000000000 ) ;
#8765 = ADVANCED_FACE ( 'NONE', ( #13474 ), #5530, .F. ) ;
#8766 = CARTESIAN_POINT ( 'NONE',  ( 78.48937290013660117, 103.1299228374914065, 220.6387154965113382 ) ) ;
#8767 = DIRECTION ( 'NONE',  ( 0.000000000000000000, 1.000000000000000000, 0.000000000000000000 ) ) ;
#8768 = DIRECTION ( 'NONE',  ( 0.000000000000000000, 0.000000000000000000, -1.000000000000000000 ) ) ;
#8769 = ADVANCED_FACE ( 'NONE', ( #6216 ), #7287, .T. ) ;
#8770 = LINE ( 'NONE', #7222, #6637 ) ;
#8771 = LINE ( 'NONE', #12934, #8572 ) ;
#8772 = CARTESIAN_POINT ( 'NONE',  ( -81.18192946989263703, 139.7545334744432637, 496.6642397995874489 ) ) ;
#8773 = EDGE_CURVE ( 'NONE', #11502, #15316, #11377, .T. ) ;
#8774 = PLANE ( 'NONE',  #15634 ) ;
#8775 = AXIS2_PLACEMENT_3D ( 'NONE', #18417, #19960, #12359 ) ;
#8776 = EDGE_LOOP ( 'NONE', ( #5228, #16040, #10743, #8536 ) ) ;
#8777 = PRESENTATION_LAYER_ASSIGNMENT (  '', '', ( #5478 ) ) ;
#8778 = ORIENTED_EDGE ( 'NONE', *, *, #18180, .T. ) ;
#8779 = ADVANCED_FACE ( 'NONE', ( #10261, #4559 ), #870, .F. ) ;
#8780 = DIRECTION ( 'NONE',  ( 0.000000000000000000, -1.000000000000000000, 0.000000000000000000 ) ) ;
#8781 = ORIENTED_EDGE ( 'NONE', *, *, #14175, .T. ) ;
#8782 = ORIENTED_EDGE ( 'NONE', *, *, #17693, .T. ) ;
#8783 = ORIENTED_EDGE ( 'NONE', *, *, #19817, .T. ) ;
#8784 =( NAMED_UNIT ( * ) SI_UNIT ( $, .STERADIAN. ) SOLID_ANGLE_UNIT ( ) );
#8785 = CARTESIAN_POINT ( 'NONE',  ( -1.000000000000001110, 216.7545334744432921, 478.3411705753777596 ) ) ;
#8786 = CARTESIAN_POINT ( 'NONE',  ( 25.99999999999999645, 68.00000000000000000, -39.99999999999999289 ) ) ;
#8787 = DIRECTION ( 'NONE',  ( 0.000000000000000000, 0.000000000000000000, -1.000000000000000000 ) ) ;
#8788 = FACE_OUTER_BOUND ( 'NONE', #11907, .T. ) ;
#8789 = LINE ( 'NONE', #17676, #19818 ) ;
#8790 = EDGE_CURVE ( 'NONE', #7147, #270, #16678, .T. ) ;
#8791 = CIRCLE ( 'NONE', #1855, 3.999999999999996447 ) ;
#8792 = CARTESIAN_POINT ( 'NONE',  ( 7.000000000000000000, 17.52499999999999858, 0.000000000000000000 ) ) ;
#8793 = CARTESIAN_POINT ( 'NONE',  ( 31.00000000000000000, 11.00000000000000000, -31.00000000000000355 ) ) ;
#8794 = CARTESIAN_POINT ( 'NONE',  ( 55.98937290013660828, 108.8727366810871899, 338.2196854716659118 ) ) ;
#8795 = DIRECTION ( 'NONE',  ( -1.000000000000000000, 0.000000000000000000, 0.000000000000000000 ) ) ;
#8796 = ORIENTED_EDGE ( 'NONE', *, *, #13100, .F. ) ;
#8797 = DIRECTION ( 'NONE',  ( 1.000000000000000000, 0.000000000000000000, 0.000000000000000000 ) ) ;
#8798 = DIRECTION ( 'NONE',  ( -3.854941057726249437E-16, 0.000000000000000000, -1.000000000000000000 ) ) ;
#8799 = EDGE_CURVE ( 'NONE', #3886, #15108, #5734, .T. ) ;
#8800 = ORIENTED_EDGE ( 'NONE', *, *, #14106, .F. ) ;
#8801 = EDGE_LOOP ( 'NONE', ( #12112, #9576 ) ) ;
#8802 = CARTESIAN_POINT ( 'NONE',  ( 31.99999999999998579, 6.000000000000000000, 21.99999999999999645 ) ) ;
#8803 = DIRECTION ( 'NONE',  ( 0.000000000000000000, 0.000000000000000000, -1.000000000000000000 ) ) ;
#8804 = ORIENTED_EDGE ( 'NONE', *, *, #11251, .F. ) ;
#8805 = PLANE ( 'NONE',  #310 ) ;
#8806 = DIRECTION ( 'NONE',  ( 0.000000000000000000, 0.000000000000000000, -1.000000000000000000 ) ) ;
#8807 = SURFACE_STYLE_FILL_AREA ( #2514 ) ;
#8808 = CARTESIAN_POINT ( 'NONE',  ( -40.00000000000000000, 19.00000000000000000, 25.99999999999999645 ) ) ;
#8809 = DIRECTION ( 'NONE',  ( -0.000000000000000000, 1.000000000000000000, -0.000000000000000000 ) ) ;
#8810 = EDGE_CURVE ( 'NONE', #12373, #1145, #12208, .T. ) ;
#8811 = DIRECTION ( 'NONE',  ( -0.000000000000000000, -0.000000000000000000, 1.000000000000000000 ) ) ;
#8812 = VECTOR ( 'NONE', #9800, 1000.000000000000000 ) ;
#8813 = ORIENTED_EDGE ( 'NONE', *, *, #5218, .F. ) ;
#8814 = DIRECTION ( 'NONE',  ( 0.000000000000000000, 1.000000000000000000, 0.000000000000000000 ) ) ;
#8815 = APPLICATION_CONTEXT ( 'automotive_design' ) ;
#8816 = DIRECTION ( 'NONE',  ( 0.000000000000000000, 0.000000000000000000, -1.000000000000000000 ) ) ;
#8817 = DIRECTION ( 'NONE',  ( 0.000000000000000000, -0.000000000000000000, -1.000000000000000000 ) ) ;
#8818 = SHAPE_DEFINITION_REPRESENTATION ( #12386, #6180 ) ;
#8819 = ORIENTED_EDGE ( 'NONE', *, *, #1563, .T. ) ;
#8820 = DIRECTION ( 'NONE',  ( 0.000000000000000000, 0.000000000000000000, -1.000000000000000000 ) ) ;
#8821 = ORIENTED_EDGE ( 'NONE', *, *, #14555, .T. ) ;
#8822 = ORIENTED_EDGE ( 'NONE', *, *, #14053, .F. ) ;
#8823 = ORIENTED_EDGE ( 'NONE', *, *, #16650, .F. ) ;
#8824 = AXIS2_PLACEMENT_3D ( 'NONE', #4784, #18774, #7863 ) ;
#8825 = DIRECTION ( 'NONE',  ( 1.000000000000000000, -0.000000000000000000, 0.000000000000000000 ) ) ;
#8826 = VERTEX_POINT ( 'NONE', #18484 ) ;
#8827 = DIRECTION ( 'NONE',  ( 1.000000000000000000, 5.889072920838430686E-16, -0.000000000000000000 ) ) ;
#8828 = CARTESIAN_POINT ( 'NONE',  ( 0.01154096739894239568, 141.3438375788570909, 501.6399373741901968 ) ) ;
#8829 = VERTEX_POINT ( 'NONE', #13562 ) ;
#8830 = LINE ( 'NONE', #15112, #4788 ) ;
#8831 = CARTESIAN_POINT ( 'NONE',  ( 153.4893729001366580, 145.9162550801369491, 250.0000000000000000 ) ) ;
#8832 = CARTESIAN_POINT ( 'NONE',  ( 37.00000000000000000, 68.00000000000000000, 23.00000000000001066 ) ) ;
#8833 = DIRECTION ( 'NONE',  ( 1.055507992432142416E-16, -0.5937146717273791285, -0.8046756418431282309 ) ) ;
#8834 = EDGE_CURVE ( 'NONE', #5632, #1294, #11054, .T. ) ;
#8835 = CARTESIAN_POINT ( 'NONE',  ( -33.99999999999997158, 3.000000000000000000, -22.99999999999999645 ) ) ;
#8836 = FILL_AREA_STYLE ('',( #18197 ) ) ;
#8837 = CARTESIAN_POINT ( 'NONE',  ( -26.00000000000002842, 3.000000000000000000, 34.00000000000000711 ) ) ;
#8838 =( NAMED_UNIT ( * ) SI_UNIT ( $, .STERADIAN. ) SOLID_ANGLE_UNIT ( ) );
#8839 =( NAMED_UNIT ( * ) SI_UNIT ( $, .STERADIAN. ) SOLID_ANGLE_UNIT ( ) );
#8840 = FACE_OUTER_BOUND ( 'NONE', #445, .T. ) ;
#8841 = DIRECTION ( 'NONE',  ( -0.000000000000000000, 0.000000000000000000, 1.000000000000000000 ) ) ;
#8842 = COLOUR_RGB ( '', 0.72549020, 0.75294118, 0.79215686) ;
#8843 = FILL_AREA_STYLE_COLOUR ( '', #13504 ) ;
#8844 = EDGE_LOOP ( 'NONE', ( #1876, #9520, #617, #3449 ) ) ;
#8845 = ORIENTED_EDGE ( 'NONE', *, *, #12080, .F. ) ;
#8846 = PRODUCT_DEFINITION_CONTEXT ( 'detailed design', #16595, 'design' ) ;
#8847 = EDGE_LOOP ( 'NONE', ( #12945, #16050, #20215, #13495 ) ) ;
#8848 = VERTEX_POINT ( 'NONE', #19820 ) ;
#8849 = EDGE_CURVE ( 'NONE', #3093, #5899, #19277, .T. ) ;
#8850 = LINE ( 'NONE', #2655, #7707 ) ;
#8851 = CYLINDRICAL_SURFACE ( 'NONE', #14815, 1.000000000000000888 ) ;
#8852 = AXIS2_PLACEMENT_3D ( 'NONE', #10556, #18281, #15406 ) ;
#8853 = LINE ( 'NONE', #13702, #14266 ) ;
#8854 = CYLINDRICAL_SURFACE ( 'NONE', #14611, 10.00000000000000888 ) ;
#8855 = DIRECTION ( 'NONE',  ( 0.000000000000000000, 0.000000000000000000, -1.000000000000000000 ) ) ;
#8856 = CARTESIAN_POINT ( 'NONE',  ( -211.5106270998635409, 113.1299228374912502, 79.58252780074349175 ) ) ;
#8857 = PRESENTATION_STYLE_ASSIGNMENT (( #7221 ) ) ;
#8858 = FILL_AREA_STYLE ('',( #2767 ) ) ;
#8859 = EDGE_CURVE ( 'NONE', #10116, #16810, #2922, .T. ) ;
#8860 = CARTESIAN_POINT ( 'NONE',  ( 458.8334540492693350, 191.8198460455371333, 81.76606011801540319 ) ) ;
#8861 = PRESENTATION_LAYER_ASSIGNMENT (  '', '', ( #13784 ) ) ;
#8862 = EDGE_CURVE ( 'NONE', #6976, #18143, #15528, .T. ) ;
#8863 = VECTOR ( 'NONE', #18908, 1000.000000000000000 ) ;
#8864 = ORIENTED_EDGE ( 'NONE', *, *, #13819, .T. ) ;
#8865 = CARTESIAN_POINT ( 'NONE',  ( -31.00000000000006395, 8.000000000000000000, 20.99999999999998934 ) ) ;
#8866 = VERTEX_POINT ( 'NONE', #6035 ) ;
#8867 = ORIENTED_EDGE ( 'NONE', *, *, #10523, .F. ) ;
#8868 = DIRECTION ( 'NONE',  ( -0.000000000000000000, -1.000000000000000000, -0.000000000000000000 ) ) ;
#8869 = UNCERTAINTY_MEASURE_WITH_UNIT (LENGTH_MEASURE( 1.000000000000000082E-05 ), #17878, 'distance_accuracy_value', 'NONE');
#8870 = CARTESIAN_POINT ( 'NONE',  ( 53.48937290013659407, 127.7247684487574588, 368.0000000000000000 ) ) ;
#8871 = ADVANCED_FACE ( 'NONE', ( #5732 ), #12314, .F. ) ;
#8872 = COLOUR_RGB ( '', 0.66274510, 0.83137255, 0.94901961) ;
#8873 = CARTESIAN_POINT ( 'NONE',  ( 463.8334540492693350, 191.8198460455371333, 81.76606011801540319 ) ) ;
#8874 = FACE_OUTER_BOUND ( 'NONE', #7817, .T. ) ;
#8875 = CARTESIAN_POINT ( 'NONE',  ( 5.950000000000000178, 0.000000000000000000, 0.000000000000000000 ) ) ;
#8876 = VECTOR ( 'NONE', #11585, 1000.000000000000000 ) ;
#8877 = CARTESIAN_POINT ( 'NONE',  ( -25.99999999999999645, 68.00000000000000000, -39.99999999999999289 ) ) ;
#8878 = CARTESIAN_POINT ( 'NONE',  ( 111.4893729001366012, 127.7247684487574304, 250.0000000000000000 ) ) ;
#8879 = DIRECTION ( 'NONE',  ( -0.000000000000000000, 1.000000000000000000, -0.000000000000000000 ) ) ;
#8880 = PLANE ( 'NONE',  #19567 ) ;
#8881 = ADVANCED_FACE ( 'NONE', ( #1246 ), #10770, .F. ) ;
#8882 = ORIENTED_EDGE ( 'NONE', *, *, #9011, .F. ) ;
#8883 = CARTESIAN_POINT ( 'NONE',  ( 31.81980515339464333, 11.00000000000000000, -31.81980515339463622 ) ) ;
#8884 = PLANE ( 'NONE',  #12991 ) ;
#8885 = DIRECTION ( 'NONE',  ( 0.000000000000000000, 0.000000000000000000, 1.000000000000000000 ) ) ;
#8886 = ADVANCED_FACE ( 'NONE', ( #9124 ), #1347, .F. ) ;
#8887 = VECTOR ( 'NONE', #13568, 1000.000000000000000 ) ;
#8888 = VECTOR ( 'NONE', #1641, 1000.000000000000000 ) ;
#8889 = ORIENTED_EDGE ( 'NONE', *, *, #910, .F. ) ;
#8890 = EDGE_CURVE ( 'NONE', #13589, #13719, #15208, .T. ) ;
#8891 = UNCERTAINTY_MEASURE_WITH_UNIT (LENGTH_MEASURE( 1.000000000000000082E-05 ), #7145, 'distance_accuracy_value', 'NONE');
#8892 = ORIENTED_EDGE ( 'NONE', *, *, #5207, .F. ) ;
#8893 = CARTESIAN_POINT ( 'NONE',  ( 53.48937290013658696, 122.8810204491430369, 280.0825295754780768 ) ) ;
#8894 = CARTESIAN_POINT ( 'NONE',  ( -36.00000000000000000, 4.408728476930470856E-15, -135.0000000000000284 ) ) ;
#8895 = UNCERTAINTY_MEASURE_WITH_UNIT (LENGTH_MEASURE( 1.000000000000000082E-05 ), #18791, 'distance_accuracy_value', 'NONE');
#8896 = ORIENTED_EDGE ( 'NONE', *, *, #4374, .F. ) ;
#8897 = PLANE ( 'NONE',  #20030 ) ;
#8898 = PRESENTATION_STYLE_ASSIGNMENT (( #11900 ) ) ;
#8899 = SURFACE_STYLE_FILL_AREA ( #16844 ) ;
#8900 = VECTOR ( 'NONE', #1511, 1000.000000000000000 ) ;
#8901 = DIRECTION ( 'NONE',  ( 0.000000000000000000, 1.000000000000000000, 0.000000000000000000 ) ) ;
#8902 = MECHANICAL_DESIGN_GEOMETRIC_PRESENTATION_REPRESENTATION (  '', ( #20064 ), #18761 ) ;
#8903 = CYLINDRICAL_SURFACE ( 'NONE', #9142, 4.999999999999997335 ) ;
#8904 = VECTOR ( 'NONE', #4669, 1000.000000000000000 ) ;
#8905 = EDGE_LOOP ( 'NONE', ( #7248, #6664, #10766, #3108 ) ) ;
#8906 = DIRECTION ( 'NONE',  ( 0.000000000000000000, 1.000000000000000000, 0.000000000000000000 ) ) ;
#8907 = DIRECTION ( 'NONE',  ( 0.000000000000000000, 0.000000000000000000, 1.000000000000000000 ) ) ;
#8908 = EDGE_LOOP ( 'NONE', ( #19080, #18947, #1693, #16671 ) ) ;
#8909 = AXIS2_PLACEMENT_3D ( 'NONE', #19565, #19457, #17824 ) ;
#8910 = ADVANCED_FACE ( 'NONE', ( #18181 ), #11919, .F. ) ;
#8911 = ORIENTED_EDGE ( 'NONE', *, *, #3613, .F. ) ;
#8912 = VERTEX_POINT ( 'NONE', #18294 ) ;
#8913 = EDGE_LOOP ( 'NONE', ( #5499, #5620, #15787, #9145 ) ) ;
#8914 = EDGE_CURVE ( 'NONE', #2877, #1858, #10667, .T. ) ;
#8915 = AXIS2_PLACEMENT_3D ( 'NONE', #5080, #15803, #7852 ) ;
#8916 = DIRECTION ( 'NONE',  ( 0.000000000000000000, 0.000000000000000000, -1.000000000000000000 ) ) ;
#8917 = ORIENTED_EDGE ( 'NONE', *, *, #10213, .T. ) ;
#8918 = CARTESIAN_POINT ( 'NONE',  ( 0.000000000000000000, -3.000000000000000888, -150.0000000000000000 ) ) ;
#8919 = CARTESIAN_POINT ( 'NONE',  ( 10.00000000000000000, 372.8685141053778693, -79.88019484660868841 ) ) ;
#8920 =( NAMED_UNIT ( * ) SI_UNIT ( $, .STERADIAN. ) SOLID_ANGLE_UNIT ( ) );
#8921 = CYLINDRICAL_SURFACE ( 'NONE', #12864, 10.00000000000000888 ) ;
#8922 = DIRECTION ( 'NONE',  ( -0.000000000000000000, -0.000000000000000000, 1.000000000000000000 ) ) ;
#8923 = SHAPE_REPRESENTATION ( 'Servo-Body', ( #2741 ), #6708 ) ;
#8924 = PRESENTATION_STYLE_ASSIGNMENT (( #10781 ) ) ;
#8925 = CARTESIAN_POINT ( 'NONE',  ( 108.9893729001366154, 95.58236431990637527, 327.6194023386000822 ) ) ;
#8926 = LINE ( 'NONE', #15221, #17381 ) ;
#8927 = CYLINDRICAL_SURFACE ( 'NONE', #9629, 2.500000000000002220 ) ;
#8928 = AXIS2_PLACEMENT_3D ( 'NONE', #6192, #12884, #14205 ) ;
#8929 = DIRECTION ( 'NONE',  ( -0.000000000000000000, 1.000000000000000000, -0.000000000000000000 ) ) ;
#8930 = CARTESIAN_POINT ( 'NONE',  ( 35.00000000000000711, 8.000000000000000000, -21.00000000000000355 ) ) ;
#8931 = SURFACE_SIDE_STYLE ('',( #18202 ) ) ;
#8932 = CARTESIAN_POINT ( 'NONE',  ( -26.00000000000000000, 11.00000000000000000, -40.00000000000000711 ) ) ;
#8933 = ORIENTED_EDGE ( 'NONE', *, *, #6780, .T. ) ;
#8934 = EDGE_LOOP ( 'NONE', ( #67, #13777, #128, #5724 ) ) ;
#8935 = ORIENTED_EDGE ( 'NONE', *, *, #18347, .T. ) ;
#8936 = EDGE_CURVE ( 'NONE', #159, #8369, #15418, .T. ) ;
#8937 = EDGE_LOOP ( 'NONE', ( #3812, #18352, #15632, #13057 ) ) ;
#8938 = DIRECTION ( 'NONE',  ( 1.000000000000000000, -0.000000000000000000, 0.000000000000000000 ) ) ;
#8939 = DIRECTION ( 'NONE',  ( 0.000000000000000000, 0.000000000000000000, 1.000000000000000000 ) ) ;
#8940 = FILL_AREA_STYLE ('',( #14378 ) ) ;
#8941 = STYLED_ITEM ( 'NONE', ( #3054 ), #8607 ) ;
#8942 = FACE_OUTER_BOUND ( 'NONE', #8981, .T. ) ;
#8943 = CARTESIAN_POINT ( 'NONE',  ( 153.4893729001366864, 123.1299228374914634, 29.36128450348865471 ) ) ;
#8944 = DIRECTION ( 'NONE',  ( 0.000000000000000000, 0.000000000000000000, 1.000000000000000000 ) ) ;
#8945 = SURFACE_STYLE_USAGE ( .BOTH. , #18522 ) ;
#8946 = DIRECTION ( 'NONE',  ( 1.000000000000000000, 9.815121534730717399E-17, 0.000000000000000000 ) ) ;
#8947 = DIRECTION ( 'NONE',  ( 1.000000000000000000, 0.000000000000000000, 0.000000000000000000 ) ) ;
#8948 = CARTESIAN_POINT ( 'NONE',  ( -3.000000000000003109, 60.00000000000000711, 9.013878188659973034 ) ) ;
#8949 = CARTESIAN_POINT ( 'NONE',  ( 25.99999999999998224, 6.000000000000000000, -31.99999999999998579 ) ) ;
#8950 = CARTESIAN_POINT ( 'NONE',  ( 111.4893729001366012, 127.7247684487574304, 252.0000000000000000 ) ) ;
#8951 = LINE ( 'NONE', #4325, #17604 ) ;
#8952 = AXIS2_PLACEMENT_3D ( 'NONE', #6391, #2689, #14103 ) ;
#8953 = CIRCLE ( 'NONE', #15553, 9.999999999999998224 ) ;
#8954 = EDGE_CURVE ( 'NONE', #8514, #4609, #16862, .T. ) ;
#8955 = VECTOR ( 'NONE', #17084, 1000.000000000000000 ) ;
#8956 = ORIENTED_EDGE ( 'NONE', *, *, #13237, .F. ) ;
#8957 = APPLICATION_CONTEXT ( 'automotive_design' ) ;
#8958 = CIRCLE ( 'NONE', #6679, 3.283624802691453848 ) ;
#8959 = LINE ( 'NONE', #13514, #16648 ) ;
#8960 = ORIENTED_EDGE ( 'NONE', *, *, #8965, .T. ) ;
#8961 = AXIS2_PLACEMENT_3D ( 'NONE', #15487, #5803, #5583 ) ;
#8962 = ORIENTED_EDGE ( 'NONE', *, *, #18444, .T. ) ;
#8963 = DIRECTION ( 'NONE',  ( 0.000000000000000000, 1.000000000000000000, 0.000000000000000000 ) ) ;
#8964 = FILL_AREA_STYLE ('',( #19981 ) ) ;
#8965 = EDGE_CURVE ( 'NONE', #14793, #16062, #2727, .T. ) ;
#8966 = CARTESIAN_POINT ( 'NONE',  ( 2.625000000000000000, 0.000000000000000000, 0.000000000000000000 ) ) ;
#8967 = AXIS2_PLACEMENT_3D ( 'NONE', #3640, #16338, #11250 ) ;
#8968 =( GEOMETRIC_REPRESENTATION_CONTEXT ( 3 ) GLOBAL_UNCERTAINTY_ASSIGNED_CONTEXT ( ( #15479 ) ) GLOBAL_UNIT_ASSIGNED_CONTEXT ( ( #11285, #5133, #462 ) ) REPRESENTATION_CONTEXT ( 'NONE', 'WORKASPACE' ) );
#8969 = FACE_OUTER_BOUND ( 'NONE', #16627, .T. ) ;
#8970 = CYLINDRICAL_SURFACE ( 'NONE', #19284, 5.000000000000004441 ) ;
#8971 = CARTESIAN_POINT ( 'NONE',  ( -78.99999999999995737, 152.4824555358011082, 486.3411705753778165 ) ) ;
#8972 = DIRECTION ( 'NONE',  ( 0.000000000000000000, 0.000000000000000000, -1.000000000000000000 ) ) ;
#8973 = ADVANCED_FACE ( 'NONE', ( #9018 ), #15321, .T. ) ;
#8974 = STYLED_ITEM ( 'NONE', ( #3867 ), #8402 ) ;
#8975 = DIRECTION ( 'NONE',  ( 0.000000000000000000, 0.000000000000000000, 1.000000000000000000 ) ) ;
#8976 =( NAMED_UNIT ( * ) PLANE_ANGLE_UNIT ( ) SI_UNIT ( $, .RADIAN. ) );
#8977 = CARTESIAN_POINT ( 'NONE',  ( -80.19446047282671941, 139.8569107142918995, 489.1724409064830184 ) ) ;
#8978 = CARTESIAN_POINT ( 'NONE',  ( 40.00000000000003553, 3.000000000000000000, 26.00000000000000355 ) ) ;
#8979 = LINE ( 'NONE', #6486, #6338 ) ;
#8980 = STYLED_ITEM ( 'NONE', ( #456 ), #3492 ) ;
#8981 = EDGE_LOOP ( 'NONE', ( #175, #1178, #10096, #15291 ) ) ;
#8982 = DIRECTION ( 'NONE',  ( 0.000000000000000000, 0.000000000000000000, 1.000000000000000000 ) ) ;
#8983 = SURFACE_STYLE_USAGE ( .BOTH. , #12091 ) ;
#8984 =( NAMED_UNIT ( * ) PLANE_ANGLE_UNIT ( ) SI_UNIT ( $, .RADIAN. ) );
#8985 = ADVANCED_FACE ( 'NONE', ( #16971 ), #4806, .F. ) ;
#8986 = AXIS2_PLACEMENT_3D ( 'NONE', #16825, #15069, #19886 ) ;
#8987 = PRESENTATION_LAYER_ASSIGNMENT (  '', '', ( #18845 ) ) ;
#8988 = ORIENTED_EDGE ( 'NONE', *, *, #15713, .T. ) ;
#8989 = EDGE_CURVE ( 'NONE', #14850, #17220, #16348, .T. ) ;
#8990 = AXIS2_PLACEMENT_3D ( 'NONE', #11646, #17819, #14526 ) ;
#8991 = EDGE_LOOP ( 'NONE', ( #18289, #10202, #18602, #1816 ) ) ;
#8992 = VECTOR ( 'NONE', #9461, 1000.000000000000000 ) ;
#8993 = LINE ( 'NONE', #18152, #7078 ) ;
#8994 = CARTESIAN_POINT ( 'NONE',  ( -3.000000000000002220, 60.00000000000000711, 6.000000000000000000 ) ) ;
#8995 = ORIENTED_EDGE ( 'NONE', *, *, #3831, .F. ) ;
#8996 = CARTESIAN_POINT ( 'NONE',  ( -20.99999999999999645, 19.00000000000000000, 35.00000000000001421 ) ) ;
#8997 = EDGE_CURVE ( 'NONE', #17019, #16028, #11173, .T. ) ;
#8998 = AXIS2_PLACEMENT_3D ( 'NONE', #2520, #16852, #4275 ) ;
#8999 =( GEOMETRIC_REPRESENTATION_CONTEXT ( 3 ) GLOBAL_UNCERTAINTY_ASSIGNED_CONTEXT ( ( #13634 ) ) GLOBAL_UNIT_ASSIGNED_CONTEXT ( ( #14941, #804, #14523 ) ) REPRESENTATION_CONTEXT ( 'NONE', 'WORKASPACE' ) );
#9000 = DIRECTION ( 'NONE',  ( -0.000000000000000000, -0.000000000000000000, 1.000000000000000000 ) ) ;
#9001 = EDGE_CURVE ( 'NONE', #16198, #11769, #19578, .T. ) ;
#9002 = DIRECTION ( 'NONE',  ( 0.000000000000000000, 0.000000000000000000, -1.000000000000000000 ) ) ;
#9003 = CARTESIAN_POINT ( 'NONE',  ( 1.181929469893224560, 140.4048636633015406, 499.8237260975782874 ) ) ;
#9004 = DIRECTION ( 'NONE',  ( 1.000000000000000000, 0.000000000000000000, 0.000000000000000000 ) ) ;
#9005 = DIRECTION ( 'NONE',  ( 0.000000000000000000, 0.000000000000000000, 1.000000000000000000 ) ) ;
#9006 = ADVANCED_FACE ( 'NONE', ( #144 ), #1128, .F. ) ;
#9007 = AXIS2_PLACEMENT_3D ( 'NONE', #1547, #3007, #7857 ) ;
#9008 = ORIENTED_EDGE ( 'NONE', *, *, #16533, .F. ) ;
#9009 = VERTEX_POINT ( 'NONE', #15832 ) ;
#9010 = DIRECTION ( 'NONE',  ( 9.815121534730717399E-17, -1.000000000000000000, 0.000000000000000000 ) ) ;
#9011 = EDGE_CURVE ( 'NONE', #12573, #13953, #5457, .T. ) ;
#9012 = ORIENTED_EDGE ( 'NONE', *, *, #16204, .T. ) ;
#9013 = ORIENTED_EDGE ( 'NONE', *, *, #10881, .T. ) ;
#9014 = ORIENTED_EDGE ( 'NONE', *, *, #5076, .T. ) ;
#9015 =( GEOMETRIC_REPRESENTATION_CONTEXT ( 3 ) GLOBAL_UNCERTAINTY_ASSIGNED_CONTEXT ( ( #14855 ) ) GLOBAL_UNIT_ASSIGNED_CONTEXT ( ( #14718, #15023, #12041 ) ) REPRESENTATION_CONTEXT ( 'NONE', 'WORKASPACE' ) );
#9016 = MECHANICAL_DESIGN_GEOMETRIC_PRESENTATION_REPRESENTATION (  '', ( #6059 ), #10665 ) ;
#9017 =( GEOMETRIC_REPRESENTATION_CONTEXT ( 3 ) GLOBAL_UNCERTAINTY_ASSIGNED_CONTEXT ( ( #14657 ) ) GLOBAL_UNIT_ASSIGNED_CONTEXT ( ( #14861, #726, #8386 ) ) REPRESENTATION_CONTEXT ( 'NONE', 'WORKASPACE' ) );
#9018 = FACE_OUTER_BOUND ( 'NONE', #2755, .T. ) ;
#9019 = COLOUR_RGB ( '', 0.40784314, 0.44705882, 0.49803922) ;
#9020 = VERTEX_POINT ( 'NONE', #1667 ) ;
#9021 = CARTESIAN_POINT ( 'NONE',  ( 0.8260971242880760235, 140.4146325554252712, 500.8352231739891067 ) ) ;
#9022 = ORIENTED_EDGE ( 'NONE', *, *, #19432, .F. ) ;
#9023 = AXIS2_PLACEMENT_3D ( 'NONE', #836, #2490, #2582 ) ;
#9024 = AXIS2_PLACEMENT_3D ( 'NONE', #17919, #3818, #10099 ) ;
#9025 = DIRECTION ( 'NONE',  ( -0.000000000000000000, -1.000000000000000000, 0.000000000000000000 ) ) ;
#9026 = CIRCLE ( 'NONE', #481, 36.00000000000000000 ) ;
#9027 = CARTESIAN_POINT ( 'NONE',  ( 0.000000000000000000, 66.00000000000000000, -9.500000000000000000 ) ) ;
#9028 = DIRECTION ( 'NONE',  ( 0.000000000000000000, 1.000000000000000000, 0.000000000000000000 ) ) ;
#9029 = SURFACE_STYLE_FILL_AREA ( #4598 ) ;
#9030 = DIRECTION ( 'NONE',  ( -0.000000000000000000, -1.000000000000000000, -0.000000000000000000 ) ) ;
#9031 = CARTESIAN_POINT ( 'NONE',  ( -78.99999999999995737, 146.1184945051222428, 479.9772095446988374 ) ) ;
#9032 = ADVANCED_FACE ( 'NONE', ( #43 ), #1566, .F. ) ;
#9033 = AXIS2_PLACEMENT_3D ( 'NONE', #9440, #15749, #4694 ) ;
#9034 = VECTOR ( 'NONE', #11654, 1000.000000000000000 ) ;
#9035 = DIRECTION ( 'NONE',  ( -0.000000000000000000, 1.000000000000000000, -0.000000000000000000 ) ) ;
#9036 = DIRECTION ( 'NONE',  ( 0.000000000000000000, -7.137148015447440312E-15, 1.000000000000000000 ) ) ;
#9037 = DIRECTION ( 'NONE',  ( -0.7976179040349734573, -1.286774331875297708E-18, -0.6031630618355673379 ) ) ;
#9038 = PRESENTATION_STYLE_ASSIGNMENT (( #13771 ) ) ;
#9039 = FACE_OUTER_BOUND ( 'NONE', #7442, .T. ) ;
#9040 = AXIS2_PLACEMENT_3D ( 'NONE', #2157, #13420, #18119 ) ;
#9041 = DIRECTION ( 'NONE',  ( -0.000000000000000000, -0.000000000000000000, 1.000000000000000000 ) ) ;
#9042 = EDGE_CURVE ( 'NONE', #19183, #16269, #4682, .T. ) ;
#9043 = FACE_OUTER_BOUND ( 'NONE', #12176, .T. ) ;
#9044 = LINE ( 'NONE', #15231, #18407 ) ;
#9045 = VERTEX_POINT ( 'NONE', #18693 ) ;
#9046 = EDGE_CURVE ( 'NONE', #6182, #14021, #3026, .T. ) ;
#9047 = VECTOR ( 'NONE', #11777, 1000.000000000000000 ) ;
#9048 = ORIENTED_EDGE ( 'NONE', *, *, #4171, .T. ) ;
#9049 = AXIS2_PLACEMENT_3D ( 'NONE', #20370, #2662, #6281 ) ;
#9050 = EDGE_LOOP ( 'NONE', ( #12789, #7033 ) ) ;
#9051 = ORIENTED_EDGE ( 'NONE', *, *, #14565, .F. ) ;
#9052 = CIRCLE ( 'NONE', #1119, 4.000000000000007105 ) ;
#9053 = PLANE ( 'NONE',  #14044 ) ;
#9054 = AXIS2_PLACEMENT_3D ( 'NONE', #4567, #9409, #19074 ) ;
#9055 = ORIENTED_EDGE ( 'NONE', *, *, #8002, .T. ) ;
#9056 =( BOUNDED_CURVE ( )  B_SPLINE_CURVE ( 3, ( #19753, #2152, #8461, #13207 ),
 .UNSPECIFIED., .F., .T. ) 
 B_SPLINE_CURVE_WITH_KNOTS ( ( 4, 4 ),
 ( 3.141592653589793116, 4.712388980384671910 ),
 .UNSPECIFIED. ) 
 CURVE ( )  GEOMETRIC_REPRESENTATION_ITEM ( )  RATIONAL_B_SPLINE_CURVE ( ( 1.000000000000000000, 0.8047378541243692673, 0.8047378541243692673, 1.000000000000000000 ) ) 
 REPRESENTATION_ITEM ( '' )  );
#9057 = CARTESIAN_POINT ( 'NONE',  ( 1.181929469891187301, 138.7545334744432637, 489.5655098179833544 ) ) ;
#9058 = CARTESIAN_POINT ( 'NONE',  ( 463.8334540492693350, 214.2156642432025251, 0.000000000000000000 ) ) ;
#9059 = CIRCLE ( 'NONE', #6112, 10.00000000000000888 ) ;
#9060 = DIRECTION ( 'NONE',  ( 9.815121534730717399E-17, -1.000000000000000000, -0.000000000000000000 ) ) ;
#9061 = ORIENTED_EDGE ( 'NONE', *, *, #7123, .F. ) ;
#9062 = SURFACE_STYLE_USAGE ( .BOTH. , #17183 ) ;
#9063 = CARTESIAN_POINT ( 'NONE',  ( 4.163799117101000559E-15, 23.00000000000000000, 34.00000000000000000 ) ) ;
#9064 = VECTOR ( 'NONE', #7905, 1000.000000000000000 ) ;
#9065 = CARTESIAN_POINT ( 'NONE',  ( 133.4893729001365443, 113.1299228374914634, 29.36128450348865471 ) ) ;
#9066 = DIRECTION ( 'NONE',  ( 4.784675105189226675E-17, 0.000000000000000000, 1.000000000000000000 ) ) ;
#9067 = SURFACE_SIDE_STYLE ('',( #15250 ) ) ;
#9068 = PRESENTATION_LAYER_ASSIGNMENT (  '', '', ( #16015 ) ) ;
#9069 = LINE ( 'NONE', #1094, #11635 ) ;
#9070 = CARTESIAN_POINT ( 'NONE',  ( 133.4893729001365728, 80.91625508013694912, 250.0000000000000000 ) ) ;
#9071 = FACE_OUTER_BOUND ( 'NONE', #8599, .T. ) ;
#9072 = EDGE_CURVE ( 'NONE', #5614, #1681, #4586, .T. ) ;
#9073 =( LENGTH_UNIT ( ) NAMED_UNIT ( * ) SI_UNIT ( .MILLI., .METRE. ) );
#9074 =( NAMED_UNIT ( * ) PLANE_ANGLE_UNIT ( ) SI_UNIT ( $, .RADIAN. ) );
#9075 = VECTOR ( 'NONE', #10217, 1000.000000000000000 ) ;
#9076 = EDGE_LOOP ( 'NONE', ( #4092, #15628, #5723, #15288 ) ) ;
#9077 = ORIENTED_EDGE ( 'NONE', *, *, #798, .T. ) ;
#9078 = ORIENTED_EDGE ( 'NONE', *, *, #4218, .T. ) ;
#9079 = DIRECTION ( 'NONE',  ( 0.000000000000000000, -1.000000000000000000, 0.000000000000000000 ) ) ;
#9080 = ORIENTED_EDGE ( 'NONE', *, *, #5922, .F. ) ;
#9081 = VERTEX_POINT ( 'NONE', #15736 ) ;
#9082 = DIRECTION ( 'NONE',  ( 0.000000000000000000, -1.000000000000000000, 0.000000000000000000 ) ) ;
#9083 = COLOUR_RGB ( '', 0.66274510, 0.83137255, 0.94901961) ;
#9084 = LINE ( 'NONE', #15374, #18863 ) ;
#9085 = UNCERTAINTY_MEASURE_WITH_UNIT (LENGTH_MEASURE( 1.000000000000000082E-05 ), #5198, 'distance_accuracy_value', 'NONE');
#9086 = CARTESIAN_POINT ( 'NONE',  ( -39.99999999999997868, -20.00000000000000000, -19.99999999999999645 ) ) ;
#9087 = SURFACE_SIDE_STYLE ('',( #10825 ) ) ;
#9088 = DIRECTION ( 'NONE',  ( 0.000000000000000000, 1.000000000000000000, 0.000000000000000000 ) ) ;
#9089 = PRODUCT_DEFINITION_SHAPE ( 'NONE', 'NONE',  #158 ) ;
#9090 = FACE_OUTER_BOUND ( 'NONE', #7357, .T. ) ;
#9091 = CARTESIAN_POINT ( 'NONE',  ( 17.99999999999998224, 10.00000000000000000, -36.99999999999999289 ) ) ;
#9092 = CARTESIAN_POINT ( 'NONE',  ( 21.99999999999998224, 10.00000000000000000, -32.99999999999999289 ) ) ;
#9093 =( NAMED_UNIT ( * ) PLANE_ANGLE_UNIT ( ) SI_UNIT ( $, .RADIAN. ) );
#9094 = AXIS2_PLACEMENT_3D ( 'NONE', #9481, #3616, #17722 ) ;
#9095 = CARTESIAN_POINT ( 'NONE',  ( -80.10292611397925100, 138.7899753264051412, 490.2690555533860106 ) ) ;
#9096 = ORIENTED_EDGE ( 'NONE', *, *, #7636, .F. ) ;
#9097 = DIRECTION ( 'NONE',  ( 0.000000000000000000, 0.000000000000000000, 1.000000000000000000 ) ) ;
#9098 =( NAMED_UNIT ( * ) PLANE_ANGLE_UNIT ( ) SI_UNIT ( $, .RADIAN. ) );
#9099 = CARTESIAN_POINT ( 'NONE',  ( -22.00000000000001776, 6.000000000000000000, 36.00000000000000711 ) ) ;
#9100 = CIRCLE ( 'NONE', #4491, 10.00000000000000888 ) ;
#9101 = ORIENTED_EDGE ( 'NONE', *, *, #10147, .T. ) ;
#9102 = EDGE_LOOP ( 'NONE', ( #7111, #17284, #676, #17513 ) ) ;
#9103 = EDGE_CURVE ( 'NONE', #8514, #6685, #14157, .T. ) ;
#9104 = DIRECTION ( 'NONE',  ( -0.000000000000000000, -1.000000000000000000, -0.000000000000000000 ) ) ;
#9105 = DIRECTION ( 'NONE',  ( -1.000000000000000000, 0.000000000000000000, -0.000000000000000000 ) ) ;
#9106 = CIRCLE ( 'NONE', #11422, 10.00000000000000888 ) ;
#9107 = ORIENTED_EDGE ( 'NONE', *, *, #17846, .T. ) ;
#9108 = LINE ( 'NONE', #20222, #15674 ) ;
#9109 = CARTESIAN_POINT ( 'NONE',  ( -80.39206744217459288, 139.5296019426642147, 500.3183257186572064 ) ) ;
#9110 = DIRECTION ( 'NONE',  ( 0.000000000000000000, 0.000000000000000000, 1.000000000000000000 ) ) ;
#9111 = CARTESIAN_POINT ( 'NONE',  ( 40.00000000000001421, 0.000000000000000000, -150.0000000000000000 ) ) ;
#9112 = CARTESIAN_POINT ( 'NONE',  ( 0.000000000000000000, 0.000000000000000000, -135.0000000000000284 ) ) ;
#9113 = ORIENTED_EDGE ( 'NONE', *, *, #11137, .F. ) ;
#9114 = CARTESIAN_POINT ( 'NONE',  ( -36.00000000000000711, 6.000000000000000000, -22.00000000000000355 ) ) ;
#9115 = APPLICATION_PROTOCOL_DEFINITION ( 'draft international standard', 'automotive_design', 1998, #18282 ) ;
#9116 = EDGE_CURVE ( 'NONE', #9147, #2723, #17259, .T. ) ;
#9117 = ORIENTED_EDGE ( 'NONE', *, *, #19714, .F. ) ;
#9118 = SURFACE_STYLE_FILL_AREA ( #5832 ) ;
#9119 = ORIENTED_EDGE ( 'NONE', *, *, #1808, .F. ) ;
#9120 = VERTEX_POINT ( 'NONE', #18895 ) ;
#9121 = ADVANCED_FACE ( 'NONE', ( #4802 ), #10083, .F. ) ;
#9122 = VERTEX_POINT ( 'NONE', #11386 ) ;
#9123 = EDGE_CURVE ( 'NONE', #13085, #5220, #3657, .T. ) ;
#9124 = FACE_OUTER_BOUND ( 'NONE', #13351, .T. ) ;
#9125 = ORIENTED_EDGE ( 'NONE', *, *, #1941, .T. ) ;
#9126 = CARTESIAN_POINT ( 'NONE',  ( -22.00000000000001776, 6.000000000000000000, 36.00000000000000711 ) ) ;
#9127 = ORIENTED_EDGE ( 'NONE', *, *, #15557, .F. ) ;
#9128 = SURFACE_SIDE_STYLE ('',( #20022 ) ) ;
#9129 = PRESENTATION_LAYER_ASSIGNMENT (  '', '', ( #10452 ) ) ;
#9130 = EDGE_CURVE ( 'NONE', #18073, #5054, #6132, .T. ) ;
#9131 = FILL_AREA_STYLE ('',( #19934 ) ) ;
#9132 = FACE_OUTER_BOUND ( 'NONE', #12575, .T. ) ;
#9133 = CYLINDRICAL_SURFACE ( 'NONE', #19345, 4.999999999999997335 ) ;
#9134 = DIRECTION ( 'NONE',  ( -1.000000000000000000, -0.000000000000000000, -0.000000000000000000 ) ) ;
#9135 = CARTESIAN_POINT ( 'NONE',  ( -39.99999999999997868, 3.000000000000000000, 26.00000000000000355 ) ) ;
#9136 = CARTESIAN_POINT ( 'NONE',  ( 25.99999999999997513, 10.00000000000000000, 31.00000000000003553 ) ) ;
#9137 = CARTESIAN_POINT ( 'NONE',  ( 34.99999999999997868, 11.00000000000000000, 40.00000000000000711 ) ) ;
#9138 = CARTESIAN_POINT ( 'NONE',  ( 53.48937290013658696, 122.8810204491430369, 280.0825295754780768 ) ) ;
#9139 = EDGE_CURVE ( 'NONE', #5220, #5629, #7122, .T. ) ;
#9140 = CARTESIAN_POINT ( 'NONE',  ( 498.8117674897343932, 191.8198460455371333, 158.2339398819845826 ) ) ;
#9141 = LINE ( 'NONE', #5759, #17422 ) ;
#9142 = AXIS2_PLACEMENT_3D ( 'NONE', #7562, #7364, #13649 ) ;
#9143 = EDGE_LOOP ( 'NONE', ( #9709, #8609, #11560, #16725, #9944, #10069, #20121, #1662, #6371, #13583, #5572, #14714, #5057, #5477, #12161, #13362, #18337, #10160, #5760, #5951, #7557, #15098, #20186, #8782, #17307, #8695, #1773, #5147 ) ) ;
#9144 = VECTOR ( 'NONE', #8623, 1000.000000000000000 ) ;
#9145 = ORIENTED_EDGE ( 'NONE', *, *, #18214, .F. ) ;
#9146 = EDGE_CURVE ( 'NONE', #6114, #9635, #4243, .T. ) ;
#9147 = VERTEX_POINT ( 'NONE', #19879 ) ;
#9148 = EDGE_LOOP ( 'NONE', ( #13558, #16893, #8640, #13202 ) ) ;
#9149 = CARTESIAN_POINT ( 'NONE',  ( -20.99999999999999645, 19.00000000000000000, -35.00000000000000711 ) ) ;
#9150 = ORIENTED_EDGE ( 'NONE', *, *, #1020, .F. ) ;
#9151 = EDGE_CURVE ( 'NONE', #17127, #15757, #20265, .T. ) ;
#9152 = LINE ( 'NONE', #13591, #3103 ) ;
#9153 = DIRECTION ( 'NONE',  ( 0.000000000000000000, 1.000000000000000000, 0.000000000000000000 ) ) ;
#9154 = ORIENTED_EDGE ( 'NONE', *, *, #10541, .F. ) ;
#9155 =( LENGTH_UNIT ( ) NAMED_UNIT ( * ) SI_UNIT ( .MILLI., .METRE. ) );
#9156 = SURFACE_STYLE_FILL_AREA ( #2860 ) ;
#9157 = FACE_OUTER_BOUND ( 'NONE', #11122, .T. ) ;
#9158 =( GEOMETRIC_REPRESENTATION_CONTEXT ( 3 ) GLOBAL_UNCERTAINTY_ASSIGNED_CONTEXT ( ( #8299 ) ) GLOBAL_UNIT_ASSIGNED_CONTEXT ( ( #6359, #259, #11283 ) ) REPRESENTATION_CONTEXT ( 'NONE', 'WORKASPACE' ) );
#9159 = LINE ( 'NONE', #10809, #8685 ) ;
#9160 = CARTESIAN_POINT ( 'NONE',  ( 37.00000000000003553, -20.00000000000000000, 20.00000000000000000 ) ) ;
#9161 =( NAMED_UNIT ( * ) SI_UNIT ( $, .STERADIAN. ) SOLID_ANGLE_UNIT ( ) );
#9162 = EDGE_CURVE ( 'NONE', #12228, #9449, #8444, .T. ) ;
#9163 = EDGE_LOOP ( 'NONE', ( #1322, #1336, #11408, #4946, #18991, #5282 ) ) ;
#9164 = VERTEX_POINT ( 'NONE', #14683 ) ;
#9165 = STYLED_ITEM ( 'NONE', ( #14762 ), #5022 ) ;
#9166 = DIRECTION ( 'NONE',  ( -0.000000000000000000, -0.000000000000000000, 1.000000000000000000 ) ) ;
#9167 = ORIENTED_EDGE ( 'NONE', *, *, #15189, .T. ) ;
#9168 = EDGE_LOOP ( 'NONE', ( #13093, #6093, #8322, #16697 ) ) ;
#9169 = ORIENTED_EDGE ( 'NONE', *, *, #1713, .F. ) ;
#9170 = CARTESIAN_POINT ( 'NONE',  ( -1.000000000000000888, 216.7545334744432921, 510.3921618609452935 ) ) ;
#9171 =( LENGTH_UNIT ( ) NAMED_UNIT ( * ) SI_UNIT ( .MILLI., .METRE. ) );
#9172 = FACE_OUTER_BOUND ( 'NONE', #1518, .T. ) ;
#9173 = DIRECTION ( 'NONE',  ( 1.000000000000000000, 0.000000000000000000, -0.000000000000000000 ) ) ;
#9174 = PLANE ( 'NONE',  #9994 ) ;
#9175 = DIRECTION ( 'NONE',  ( -0.000000000000000000, -0.000000000000000000, 1.000000000000000000 ) ) ;
#9176 =( NAMED_UNIT ( * ) SI_UNIT ( $, .STERADIAN. ) SOLID_ANGLE_UNIT ( ) );
#9177 = FILL_AREA_STYLE ('',( #7841 ) ) ;
#9178 = AXIS2_PLACEMENT_3D ( 'NONE', #20296, #18747, #11040 ) ;
#9179 = CARTESIAN_POINT ( 'NONE',  ( 0.9999999999997842837, 139.4861549369088323, 500.2186618848270996 ) ) ;
#9180 = ORIENTED_EDGE ( 'NONE', *, *, #1221, .T. ) ;
#9181 = DIRECTION ( 'NONE',  ( 1.000000000000000000, 0.000000000000000000, 0.000000000000000000 ) ) ;
#9182 = DIRECTION ( 'NONE',  ( -0.000000000000000000, -1.000000000000000000, 0.000000000000000000 ) ) ;
#9183 = PRESENTATION_STYLE_ASSIGNMENT (( #9401 ) ) ;
#9184 = VERTEX_POINT ( 'NONE', #10516 ) ;
#9185 =( REPRESENTATION_RELATIONSHIP ('NONE','NONE', #13279, #16597 ) REPRESENTATION_RELATIONSHIP_WITH_TRANSFORMATION ( #16139 )SHAPE_REPRESENTATION_RELATIONSHIP( ) );
#9186 = EDGE_CURVE ( 'NONE', #10424, #14402, #2188, .T. ) ;
#9187 = PRESENTATION_LAYER_ASSIGNMENT (  '', '', ( #14467 ) ) ;
#9188 = DIRECTION ( 'NONE',  ( -0.000000000000000000, -1.000000000000000000, -0.000000000000000000 ) ) ;
#9190 = ORIENTED_EDGE ( 'NONE', *, *, #14538, .T. ) ;
#9189 = STYLED_ITEM ( 'NONE', ( #18998 ), #10903 ) ;
#9191 = CARTESIAN_POINT ( 'NONE',  ( 21.00000000000000000, 8.000000000000000000, 31.00000000000006395 ) ) ;
#9192 = CARTESIAN_POINT ( 'NONE',  ( 3.850000000000000089, 0.000000000000000000, 0.000000000000000000 ) ) ;
#9193 = ORIENTED_EDGE ( 'NONE', *, *, #9602, .T. ) ;
#9194 = DIRECTION ( 'NONE',  ( 1.000000000000000000, 0.000000000000000000, -0.000000000000000000 ) ) ;
#9195 = FILL_AREA_STYLE ('',( #20319 ) ) ;
#9196 = CARTESIAN_POINT ( 'NONE',  ( -26.00000000000002842, 0.000000000000000000, -39.99999999999999289 ) ) ;
#9197 = DIRECTION ( 'NONE',  ( 0.000000000000000000, 1.000000000000000000, -0.000000000000000000 ) ) ;
#9198 = LINE ( 'NONE', #3012, #1634 ) ;
#9199 = LINE ( 'NONE', #20229, #486 ) ;
#9200 = ORIENTED_EDGE ( 'NONE', *, *, #2109, .F. ) ;
#9201 = CARTESIAN_POINT ( 'NONE',  ( -211.5106270998635409, 113.1299228374912502, 29.36128450348865471 ) ) ;
#9202 = ORIENTED_EDGE ( 'NONE', *, *, #18355, .T. ) ;
#9203 = CARTESIAN_POINT ( 'NONE',  ( -18.00000000000001421, 6.000000000000000000, 36.00000000000000711 ) ) ;
#9204 = CIRCLE ( 'NONE', #8543, 1.000000000000000888 ) ;
#9205 = ITEM_DEFINED_TRANSFORMATION ( 'NONE', 'NONE', #1408,  #2741 ) ;
#9206 = VECTOR ( 'NONE', #19255, 1000.000000000000000 ) ;
#9207 = CIRCLE ( 'NONE', #2278, 10.00000000000000178 ) ;
#9208 = ORIENTED_EDGE ( 'NONE', *, *, #20246, .F. ) ;
#9209 = ORIENTED_EDGE ( 'NONE', *, *, #19571, .T. ) ;
#9210 = CARTESIAN_POINT ( 'NONE',  ( 0.000000000000000000, 5.000000000000000888, -150.0000000000000000 ) ) ;
#9211 = ADVANCED_FACE ( 'NONE', ( #3757 ), #14567, .F. ) ;
#9212 = EDGE_LOOP ( 'NONE', ( #16956, #12036, #19617, #14866 ) ) ;
#9213 = ORIENTED_EDGE ( 'NONE', *, *, #7765, .F. ) ;
#9214 = EDGE_LOOP ( 'NONE', ( #16784, #1500, #5570, #17020, #15419, #9908, #9375, #6543 ) ) ;
#9215 = CARTESIAN_POINT ( 'NONE',  ( 17.99999999999998224, 6.000000000000000000, -35.99999999999999289 ) ) ;
#9216 = EDGE_LOOP ( 'NONE', ( #19350, #12258, #10049, #2147 ) ) ;
#9217 = CARTESIAN_POINT ( 'NONE',  ( 0.9116948254154977338, 140.4048636633015406, 500.8237260975782874 ) ) ;
#9218 = STYLED_ITEM ( 'NONE', ( #815 ), #16547 ) ;
#9219 = AXIS2_PLACEMENT_3D ( 'NONE', #5655, #5554, #13592 ) ;
#9220 = FACE_OUTER_BOUND ( 'NONE', #14821, .T. ) ;
#9221 = COLOUR_RGB ( '', 0.66274510, 0.83137255, 0.94901961) ;
#9222 = EDGE_CURVE ( 'NONE', #10544, #9619, #17670, .T. ) ;
#9223 = CIRCLE ( 'NONE', #5567, 1.000000000000000888 ) ;
#9224 = CARTESIAN_POINT ( 'NONE',  ( -211.5106270998635409, 103.1299228374912360, 170.4174721992565082 ) ) ;
#9225 = DIRECTION ( 'NONE',  ( 0.000000000000000000, 0.000000000000000000, -1.000000000000000000 ) ) ;
#9226 = CARTESIAN_POINT ( 'NONE',  ( 143.0892156028631348, 167.9162550801369491, 250.0000000000000000 ) ) ;
#9227 = DIRECTION ( 'NONE',  ( 0.000000000000000000, 1.000000000000000000, 0.000000000000000000 ) ) ;
#9228 = EDGE_CURVE ( 'NONE', #19977, #658, #2160, .T. ) ;
#9229 = DIRECTION ( 'NONE',  ( 0.000000000000000000, 0.000000000000000000, -1.000000000000000000 ) ) ;
#9230 = CARTESIAN_POINT ( 'NONE',  ( 98.48937290013662960, 113.1299228374914350, 29.36128450348865471 ) ) ;
#9231 = FACE_OUTER_BOUND ( 'NONE', #554, .T. ) ;
#9232 = DIRECTION ( 'NONE',  ( -0.000000000000000000, -0.000000000000000000, 1.000000000000000000 ) ) ;
#9233 = CARTESIAN_POINT ( 'NONE',  ( -37.00000000000000711, 10.00000000000000000, -23.00000000000000000 ) ) ;
#9234 = FACE_OUTER_BOUND ( 'NONE', #7550, .T. ) ;
#9235 = SURFACE_STYLE_USAGE ( .BOTH. , #10791 ) ;
#9236 = CIRCLE ( 'NONE', #10549, 3.000000000000002665 ) ;
#9237 = EDGE_CURVE ( 'NONE', #20154, #8032, #10407, .T. ) ;
#9238 = ADVANCED_FACE ( 'NONE', ( #644 ), #19308, .T. ) ;
#9239 = VERTEX_POINT ( 'NONE', #10047 ) ;
#9240 = PRODUCT_DEFINITION_SHAPE ( 'NONE', 'NONE',  #14766 ) ;
#9241 = ORIENTED_EDGE ( 'NONE', *, *, #2608, .T. ) ;
#9242 = PLANE ( 'NONE',  #12571 ) ;
#9243 = VERTEX_POINT ( 'NONE', #5209 ) ;
#9244 = DIRECTION ( 'NONE',  ( 0.000000000000000000, 0.000000000000000000, -1.000000000000000000 ) ) ;
#9245 = EDGE_CURVE ( 'NONE', #10116, #11471, #1494, .T. ) ;
#9246 = FACE_OUTER_BOUND ( 'NONE', #16247, .T. ) ;
#9247 = ORIENTED_EDGE ( 'NONE', *, *, #14957, .F. ) ;
#9248 = AXIS2_PLACEMENT_3D ( 'NONE', #16166, #1993, #6083 ) ;
#9249 = AXIS2_PLACEMENT_3D ( 'NONE', #2336, #2019, #8341 ) ;
#9250 = CARTESIAN_POINT ( 'NONE',  ( 25.99999999999998224, 10.00000000000000000, -31.00000000000003197 ) ) ;
#9251 = AXIS2_PLACEMENT_3D ( 'NONE', #5986, #4156, #12082 ) ;
#9252 = CARTESIAN_POINT ( 'NONE',  ( 31.99999999999998579, 6.000000000000000000, 25.99999999999999645 ) ) ;
#9253 = SURFACE_SIDE_STYLE ('',( #1602 ) ) ;
#9254 = PRESENTATION_STYLE_ASSIGNMENT (( #7430 ) ) ;
#9255 = FACE_OUTER_BOUND ( 'NONE', #5050, .T. ) ;
#9256 = PRESENTATION_STYLE_ASSIGNMENT (( #6389 ) ) ;
#9257 = EDGE_CURVE ( 'NONE', #1902, #9830, #16727, .T. ) ;
#9258 = FILL_AREA_STYLE_COLOUR ( '', #12879 ) ;
#9259 = DIRECTION ( 'NONE',  ( 0.000000000000000000, 0.000000000000000000, 1.000000000000000000 ) ) ;
#9260 = EDGE_CURVE ( 'NONE', #4676, #4285, #12711, .T. ) ;
#9261 = ADVANCED_FACE ( 'NONE', ( #8198, #17764, #5409, #14470, #346 ), #11694, .F. ) ;
#9262 = EDGE_LOOP ( 'NONE', ( #118, #12579, #6345, #7289 ) ) ;
#9263 = AXIS2_PLACEMENT_3D ( 'NONE', #13556, #9010, #13661 ) ;
#9264 = VERTEX_POINT ( 'NONE', #9170 ) ;
#9265 = ORIENTED_EDGE ( 'NONE', *, *, #18188, .T. ) ;
#9266 = ORIENTED_EDGE ( 'NONE', *, *, #13907, .F. ) ;
#9267 = VECTOR ( 'NONE', #19422, 1000.000000000000000 ) ;
#9268 = ORIENTED_EDGE ( 'NONE', *, *, #17446, .F. ) ;
#9269 = VERTEX_POINT ( 'NONE', #14113 ) ;
#9270 = ORIENTED_EDGE ( 'NONE', *, *, #1808, .T. ) ;
#9271 = CARTESIAN_POINT ( 'NONE',  ( 0.000000000000000000, 66.00000000000000000, 0.000000000000000000 ) ) ;
#9272 = CARTESIAN_POINT ( 'NONE',  ( 0.000000000000000000, 0.000000000000000000, 250.0000000000000000 ) ) ;
#9273 = DIRECTION ( 'NONE',  ( 0.000000000000000000, 0.000000000000000000, 1.000000000000000000 ) ) ;
#9274 = FILL_AREA_STYLE ('',( #4857 ) ) ;
#9275 = DIRECTION ( 'NONE',  ( 0.000000000000000000, 0.000000000000000000, -1.000000000000000000 ) ) ;
#9276 = EDGE_LOOP ( 'NONE', ( #14063, #14423 ) ) ;
#9277 = PRESENTATION_STYLE_ASSIGNMENT (( #18546 ) ) ;
#9278 = CARTESIAN_POINT ( 'NONE',  ( 35.99999999999999289, 8.000000000000000000, 18.99999999999999289 ) ) ;
#9279 = STYLED_ITEM ( 'NONE', ( #20035 ), #18050 ) ;
#9280 = CARTESIAN_POINT ( 'NONE',  ( 34.00000000000002842, -20.00000000000000000, 23.00000000000000355 ) ) ;
#9281 = CYLINDRICAL_SURFACE ( 'NONE', #16180, 10.00000000000001066 ) ;
#9282 = DIRECTION ( 'NONE',  ( -1.000000000000000000, -0.000000000000000000, -0.000000000000000000 ) ) ;
#9283 = ORIENTED_EDGE ( 'NONE', *, *, #12347, .F. ) ;
#9284 = DIRECTION ( 'NONE',  ( 0.000000000000000000, 1.000000000000000000, 0.000000000000000000 ) ) ;
#9285 = FILL_AREA_STYLE_COLOUR ( '', #15284 ) ;
#9286 = ADVANCED_FACE ( 'NONE', ( #12476 ), #19979, .T. ) ;
#9287 = CARTESIAN_POINT ( 'NONE',  ( 1.469576158976824144E-15, 0.000000000000000000, 12.00000000000000178 ) ) ;
#9288 = AXIS2_PLACEMENT_3D ( 'NONE', #19724, #20136, #5743 ) ;
#9289 = EDGE_CURVE ( 'NONE', #7627, #9009, #10934, .T. ) ;
#9290 = EDGE_LOOP ( 'NONE', ( #13448, #20078, #11462, #14391 ) ) ;
#9291 = AXIS2_PLACEMENT_3D ( 'NONE', #15225, #786, #16586 ) ;
#9292 = VECTOR ( 'NONE', #9638, 1000.000000000000000 ) ;
#9293 = VECTOR ( 'NONE', #12768, 1000.000000000000000 ) ;
#9294 = SURFACE_STYLE_USAGE ( .BOTH. , #7650 ) ;
#9295 = ORIENTED_EDGE ( 'NONE', *, *, #19712, .F. ) ;
#9296 =( LENGTH_UNIT ( ) NAMED_UNIT ( * ) SI_UNIT ( .MILLI., .METRE. ) );
#9297 =( LENGTH_UNIT ( ) NAMED_UNIT ( * ) SI_UNIT ( .MILLI., .METRE. ) );
#9298 = ORIENTED_EDGE ( 'NONE', *, *, #14794, .T. ) ;
#9299 = FACE_OUTER_BOUND ( 'NONE', #86, .T. ) ;
#9300 = CARTESIAN_POINT ( 'NONE',  ( 45.00000000000001421, 0.000000000000000000, -150.0000000000000000 ) ) ;
#9301 = FACE_OUTER_BOUND ( 'NONE', #5586, .T. ) ;
#9302 = CIRCLE ( 'NONE', #3727, 3.000000000000009770 ) ;
#9303 = VECTOR ( 'NONE', #6511, 1000.000000000000000 ) ;
#9304 = CARTESIAN_POINT ( 'NONE',  ( -0.4029650338733730131, 139.7904024160982033, 500.8581393444502510 ) ) ;
#9305 = CARTESIAN_POINT ( 'NONE',  ( 25.99999999999996092, 3.000000000000000000, 31.00000000000004263 ) ) ;
#9306 = DIRECTION ( 'NONE',  ( -0.000000000000000000, 1.000000000000000000, 0.000000000000000000 ) ) ;
#9307 = CARTESIAN_POINT ( 'NONE',  ( 53.48937290013659407, 49.66333933884487806, 252.0000000000000000 ) ) ;
#9308 = ORIENTED_EDGE ( 'NONE', *, *, #19223, .F. ) ;
#9309 = CARTESIAN_POINT ( 'NONE',  ( 0.000000000000000000, -3.000000000000000888, -150.0000000000000000 ) ) ;
#9310 = PLANE ( 'NONE',  #15176 ) ;
#9311 = VECTOR ( 'NONE', #5196, 1000.000000000000000 ) ;
#9312 = VECTOR ( 'NONE', #7297, 1000.000000000000000 ) ;
#9313 = CARTESIAN_POINT ( 'NONE',  ( 149.0892156028631348, 80.91625508013694912, 245.0000000000000000 ) ) ;
#9314 = ADVANCED_FACE ( 'NONE', ( #9384 ), #18540, .T. ) ;
#9315 = VERTEX_POINT ( 'NONE', #3384 ) ;
#9316 = ORIENTED_EDGE ( 'NONE', *, *, #11779, .T. ) ;
#9317 = CARTESIAN_POINT ( 'NONE',  ( 0.000000000000000000, 0.000000000000000000, 245.0000000000000000 ) ) ;
#9318 = ORIENTED_EDGE ( 'NONE', *, *, #6885, .F. ) ;
#9319 = ORIENTED_EDGE ( 'NONE', *, *, #914, .F. ) ;
#9320 = CIRCLE ( 'NONE', #11292, 4.999999999999997335 ) ;
#9321 = EDGE_LOOP ( 'NONE', ( #5861, #7958, #10067, #3608 ) ) ;
#9322 = DIRECTION ( 'NONE',  ( -0.000000000000000000, -1.000000000000000000, -0.000000000000000000 ) ) ;
#9323 = ORIENTED_EDGE ( 'NONE', *, *, #14911, .T. ) ;
#9324 = SURFACE_STYLE_FILL_AREA ( #1670 ) ;
#9325 = AXIS2_PLACEMENT_3D ( 'NONE', #10761, #16958, #8817 ) ;
#9326 = CARTESIAN_POINT ( 'NONE',  ( 423.8334540492694487, 191.8198460455371333, 24.99421986894476078 ) ) ;
#9327 = SURFACE_STYLE_FILL_AREA ( #18701 ) ;
#9328 = CARTESIAN_POINT ( 'NONE',  ( -80.36109718184712847, 139.8077570230245783, 489.3462760475625828 ) ) ;
#9329 = DIRECTION ( 'NONE',  ( 0.000000000000000000, -1.000000000000000000, 0.000000000000000000 ) ) ;
#9330 = DIRECTION ( 'NONE',  ( -1.000000000000000000, -0.000000000000000000, -0.000000000000000000 ) ) ;
#9331 =( GEOMETRIC_REPRESENTATION_CONTEXT ( 3 ) GLOBAL_UNCERTAINTY_ASSIGNED_CONTEXT ( ( #19795 ) ) GLOBAL_UNIT_ASSIGNED_CONTEXT ( ( #15422, #7579, #13863 ) ) REPRESENTATION_CONTEXT ( 'NONE', 'WORKASPACE' ) );
#9332 = DIRECTION ( 'NONE',  ( 1.000000000000000000, 0.000000000000000000, 0.000000000000000000 ) ) ;
#9333 = AXIS2_PLACEMENT_3D ( 'NONE', #9272, #4336, #18341 ) ;
#9334 = EDGE_LOOP ( 'NONE', ( #5857, #8663 ) ) ;
#9335 = FACE_OUTER_BOUND ( 'NONE', #15346, .T. ) ;
#9336 =( NAMED_UNIT ( * ) SI_UNIT ( $, .STERADIAN. ) SOLID_ANGLE_UNIT ( ) );
#9337 = CARTESIAN_POINT ( 'NONE',  ( -78.99999999999995737, 140.8764026050586722, 502.4686618848272133 ) ) ;
#9338 = CARTESIAN_POINT ( 'NONE',  ( -20.99999999999999645, 8.000000000000000000, -31.00000000000003553 ) ) ;
#9339 = DIRECTION ( 'NONE',  ( 0.000000000000000000, 0.000000000000000000, -1.000000000000000000 ) ) ;
#9340 = CARTESIAN_POINT ( 'NONE',  ( 111.4893729001366012, 127.7247684487574588, 254.0000000000000000 ) ) ;
#9341 = STYLED_ITEM ( 'NONE', ( #4012 ), #12135 ) ;
#9342 = VECTOR ( 'NONE', #13628, 1000.000000000000000 ) ;
#9343 =( GEOMETRIC_REPRESENTATION_CONTEXT ( 3 ) GLOBAL_UNCERTAINTY_ASSIGNED_CONTEXT ( ( #4173 ) ) GLOBAL_UNIT_ASSIGNED_CONTEXT ( ( #17002, #10491, #18415 ) ) REPRESENTATION_CONTEXT ( 'NONE', 'WORKASPACE' ) );
#9344 =( GEOMETRIC_REPRESENTATION_CONTEXT ( 3 ) GLOBAL_UNCERTAINTY_ASSIGNED_CONTEXT ( ( #11768 ) ) GLOBAL_UNIT_ASSIGNED_CONTEXT ( ( #7591, #1487, #10889 ) ) REPRESENTATION_CONTEXT ( 'NONE', 'WORKASPACE' ) );
#9345 = EDGE_CURVE ( 'NONE', #1376, #18127, #189, .T. ) ;
#9346 = VERTEX_POINT ( 'NONE', #16916 ) ;
#9347 = AXIS2_PLACEMENT_3D ( 'NONE', #14448, #11464, #17843 ) ;
#9348 = PRESENTATION_LAYER_ASSIGNMENT (  '', '', ( #2429 ) ) ;
#9349 = PRODUCT_DEFINITION ( 'UNKNOWN', '', #14900, #7411 ) ;
#9350 = ORIENTED_EDGE ( 'NONE', *, *, #8426, .F. ) ;
#9351 = DIRECTION ( 'NONE',  ( 0.000000000000000000, 1.000000000000000000, 0.000000000000000000 ) ) ;
#9352 = PLANE ( 'NONE',  #5819 ) ;
#9353 = AXIS2_PLACEMENT_3D ( 'NONE', #15639, #10977, #7793 ) ;
#9354 = ORIENTED_EDGE ( 'NONE', *, *, #5396, .T. ) ;
#9355 = CARTESIAN_POINT ( 'NONE',  ( 153.4893729001366864, 113.1299228374914634, 220.6387154965113382 ) ) ;
#9356 = CARTESIAN_POINT ( 'NONE',  ( 498.8334540492693918, 167.8734308960555950, 0.000000000000000000 ) ) ;
#9357 = ORIENTED_EDGE ( 'NONE', *, *, #3518, .T. ) ;
#9358 = EDGE_CURVE ( 'NONE', #12917, #15939, #5468, .T. ) ;
#9359 = ADVANCED_BREP_SHAPE_REPRESENTATION ( '', ( #2209, #2741 ), #4683 ) ;
#9360 =( GEOMETRIC_REPRESENTATION_CONTEXT ( 3 ) GLOBAL_UNCERTAINTY_ASSIGNED_CONTEXT ( ( #17740 ) ) GLOBAL_UNIT_ASSIGNED_CONTEXT ( ( #6357, #16981, #12638 ) ) REPRESENTATION_CONTEXT ( 'NONE', 'WORKASPACE' ) );
#9361 = AXIS2_PLACEMENT_3D ( 'NONE', #8860, #19568, #18027 ) ;
#9362 = AXIS2_PLACEMENT_3D ( 'NONE', #2810, #20004, #4064 ) ;
#9363 = LINE ( 'NONE', #12459, #7093 ) ;
#9364 = DIRECTION ( 'NONE',  ( -1.000000000000000000, -8.479266908829339085E-16, 0.000000000000000000 ) ) ;
#9365 = CARTESIAN_POINT ( 'NONE',  ( -38.50085094405407204, 209.4098724938429541, 505.3921618609452935 ) ) ;
#9366 = DIRECTION ( 'NONE',  ( 0.000000000000000000, 0.000000000000000000, -1.000000000000000000 ) ) ;
#9367 = CARTESIAN_POINT ( 'NONE',  ( 40.00000000000001421, 0.000000000000000000, 0.000000000000000000 ) ) ;
#9368 = VECTOR ( 'NONE', #15472, 1000.000000000000000 ) ;
#9369 = VECTOR ( 'NONE', #10074, 1000.000000000000000 ) ;
#9370 = FACE_OUTER_BOUND ( 'NONE', #18814, .T. ) ;
#9371 = PRESENTATION_STYLE_ASSIGNMENT (( #4844 ) ) ;
#9372 = MECHANICAL_DESIGN_GEOMETRIC_PRESENTATION_REPRESENTATION (  '', ( #6088 ), #11026 ) ;
#9373 = EDGE_CURVE ( 'NONE', #14625, #18451, #2780, .T. ) ;
#9374 = EDGE_CURVE ( 'NONE', #2287, #6649, #14024, .T. ) ;
#9375 = ORIENTED_EDGE ( 'NONE', *, *, #3577, .F. ) ;
#9376 = ORIENTED_EDGE ( 'NONE', *, *, #4304, .T. ) ;
#9377 = PRESENTATION_LAYER_ASSIGNMENT (  '', '', ( #1450 ) ) ;
#9378 = EDGE_LOOP ( 'NONE', ( #9792, #8732, #17865, #2999 ) ) ;
#9379 = EDGE_CURVE ( 'NONE', #4219, #18458, #8100, .T. ) ;
#9380 = CARTESIAN_POINT ( 'NONE',  ( -22.99999999999999645, 0.000000000000000000, -31.00000000000005684 ) ) ;
#9381 = VERTEX_POINT ( 'NONE', #11038 ) ;
#9382 = ORIENTED_EDGE ( 'NONE', *, *, #14045, .T. ) ;
#9383 = VERTEX_POINT ( 'NONE', #15584 ) ;
#9384 = FACE_OUTER_BOUND ( 'NONE', #5430, .T. ) ;
#9385 = EDGE_CURVE ( 'NONE', #3638, #1247, #2677, .T. ) ;
#9386 = AXIS2_PLACEMENT_3D ( 'NONE', #1950, #222, #8266 ) ;
#9387 =( NAMED_UNIT ( * ) SI_UNIT ( $, .STERADIAN. ) SOLID_ANGLE_UNIT ( ) );
#9388 = VECTOR ( 'NONE', #3030, 1000.000000000000000 ) ;
#9389 =( NAMED_UNIT ( * ) SI_UNIT ( $, .STERADIAN. ) SOLID_ANGLE_UNIT ( ) );
#9390 = ADVANCED_FACE ( 'NONE', ( #20187 ), #10725, .F. ) ;
#9391 = FILL_AREA_STYLE ('',( #4648 ) ) ;
#9392 = LINE ( 'NONE', #12580, #14929 ) ;
#9393 = PLANE ( 'NONE',  #7345 ) ;
#9394 = EDGE_CURVE ( 'NONE', #7608, #6545, #17021, .T. ) ;
#9395 = CARTESIAN_POINT ( 'NONE',  ( -34.99999999999998579, -20.00000000000000000, 23.50000000000000711 ) ) ;
#9396 = LINE ( 'NONE', #20200, #1711 ) ;
#9397 = CARTESIAN_POINT ( 'NONE',  ( 10.00000000000000000, 381.0487089519826895, 2.719601036885452502E-12 ) ) ;
#9398 = VECTOR ( 'NONE', #9000, 1000.000000000000000 ) ;
#9399 = ORIENTED_EDGE ( 'NONE', *, *, #905, .F. ) ;
#9400 = CARTESIAN_POINT ( 'NONE',  ( -40.00000000000000711, 8.000000000000000000, -19.00000000000000355 ) ) ;
#9401 = SURFACE_STYLE_USAGE ( .BOTH. , #1746 ) ;
#9402 = ADVANCED_FACE ( 'NONE', ( #10822 ), #17499, .T. ) ;
#9403 = MECHANICAL_DESIGN_GEOMETRIC_PRESENTATION_REPRESENTATION (  '', ( #11706 ), #7760 ) ;
#9404 = ORIENTED_EDGE ( 'NONE', *, *, #17057, .F. ) ;
#9405 = VERTEX_POINT ( 'NONE', #15886 ) ;
#9406 = EDGE_CURVE ( 'NONE', #6967, #16566, #8351, .T. ) ;
#9407 = EDGE_LOOP ( 'NONE', ( #8151, #12133, #5285, #17939 ) ) ;
#9408 = AXIS2_PLACEMENT_3D ( 'NONE', #8158, #3409, #17629 ) ;
#9409 = DIRECTION ( 'NONE',  ( 0.000000000000000000, -0.7071067811865455743, -0.7071067811865494601 ) ) ;
#9410 = ADVANCED_FACE ( 'NONE', ( #3295 ), #16104, .T. ) ;
#9411 = AXIS2_PLACEMENT_3D ( 'NONE', #12263, #20079, #12378 ) ;
#9412 = FILL_AREA_STYLE ('',( #17241 ) ) ;
#9413 = DIRECTION ( 'NONE',  ( -0.000000000000000000, -0.000000000000000000, 1.000000000000000000 ) ) ;
#9414 = CYLINDRICAL_SURFACE ( 'NONE', #1289, 4.999999999999997335 ) ;
#9415 = PRESENTATION_STYLE_ASSIGNMENT (( #4670 ) ) ;
#9416 = EDGE_LOOP ( 'NONE', ( #20012, #4376, #7601, #12547 ) ) ;
#9417 = PLANE ( 'NONE',  #5884 ) ;
#9418 = DIRECTION ( 'NONE',  ( -0.000000000000000000, 1.000000000000000000, -0.000000000000000000 ) ) ;
#9419 = CARTESIAN_POINT ( 'NONE',  ( 40.00000000000000711, 8.000000000000000000, 34.99999999999997868 ) ) ;
#9420 = PRODUCT_DEFINITION_SHAPE ( 'NONE', 'NONE',  #13275 ) ;
#9421 = ORIENTED_EDGE ( 'NONE', *, *, #1834, .T. ) ;
#9422 = ORIENTED_EDGE ( 'NONE', *, *, #11008, .T. ) ;
#9423 =( NAMED_UNIT ( * ) PLANE_ANGLE_UNIT ( ) SI_UNIT ( $, .RADIAN. ) );
#9424 = ORIENTED_EDGE ( 'NONE', *, *, #2906, .F. ) ;
#9425 = VERTEX_POINT ( 'NONE', #13003 ) ;
#9426 = COLOUR_RGB ( '', 0.08235294, 0.09019608, 0.10196078) ;
#9427 = EDGE_CURVE ( 'NONE', #14904, #6321, #13381, .T. ) ;
#9428 = VERTEX_POINT ( 'NONE', #7934 ) ;
#9429 = VECTOR ( 'NONE', #2316, 1000.000000000000000 ) ;
#9430 = DIRECTION ( 'NONE',  ( -0.000000000000000000, -1.000000000000000000, -0.000000000000000000 ) ) ;
#9431 = EDGE_LOOP ( 'NONE', ( #4047, #14372, #15414, #11748 ) ) ;
#9432 = CARTESIAN_POINT ( 'NONE',  ( 88.88953019741013861, 80.91625508013694912, 250.0000000000000000 ) ) ;
#9433 = VERTEX_POINT ( 'NONE', #11438 ) ;
#9434 = LINE ( 'NONE', #13973, #10368 ) ;
#9435 = DIRECTION ( 'NONE',  ( 0.000000000000000000, 0.000000000000000000, 1.000000000000000000 ) ) ;
#9436 =( NAMED_UNIT ( * ) SI_UNIT ( $, .STERADIAN. ) SOLID_ANGLE_UNIT ( ) );
#9437 = DIRECTION ( 'NONE',  ( 1.000000000000000000, 0.000000000000000000, 0.000000000000000000 ) ) ;
#9438 = PRESENTATION_STYLE_ASSIGNMENT (( #3252 ) ) ;
#9439 = DIRECTION ( 'NONE',  ( 1.000000000000000000, 0.000000000000000000, 0.000000000000000000 ) ) ;
#9440 = CARTESIAN_POINT ( 'NONE',  ( -21.85283368562565443, 317.7545334744432353, 485.1700099148404774 ) ) ;
#9441 = ORIENTED_EDGE ( 'NONE', *, *, #1476, .T. ) ;
#9442 = DIRECTION ( 'NONE',  ( 0.000000000000000000, 0.000000000000000000, -1.000000000000000000 ) ) ;
#9443 = PLANE ( 'NONE',  #16553 ) ;
#9444 = CARTESIAN_POINT ( 'NONE',  ( -79.99999999999995737, 216.7545334744432921, 488.5655098179835818 ) ) ;
#9445 = DIRECTION ( 'NONE',  ( 1.000000000000000000, 0.000000000000000000, -0.000000000000000000 ) ) ;
#9446 = DIRECTION ( 'NONE',  ( -0.000000000000000000, -1.000000000000000000, 0.000000000000000000 ) ) ;
#9447 =( LENGTH_UNIT ( ) NAMED_UNIT ( * ) SI_UNIT ( .MILLI., .METRE. ) );
#9448 = CARTESIAN_POINT ( 'NONE',  ( -21.00000000000002842, 3.000000000000000000, -34.99999999999999289 ) ) ;
#9449 = VERTEX_POINT ( 'NONE', #1730 ) ;
#9450 = CIRCLE ( 'NONE', #1196, 1.000000000000000888 ) ;
#9451 = VERTEX_POINT ( 'NONE', #8040 ) ;
#9452 = CARTESIAN_POINT ( 'NONE',  ( -31.00000000000002132, 0.000000000000000000, -31.00000000000000000 ) ) ;
#9453 = CARTESIAN_POINT ( 'NONE',  ( -79.89735735534783601, 140.5749758762136423, 502.0985609692173739 ) ) ;
#9454 = VERTEX_POINT ( 'NONE', #3513 ) ;
#9455 = CARTESIAN_POINT ( 'NONE',  ( -211.5106270998635409, 123.1299228374912644, 79.58252780074349175 ) ) ;
#9456 = EDGE_CURVE ( 'NONE', #19242, #6358, #6710, .T. ) ;
#9457 = CARTESIAN_POINT ( 'NONE',  ( -80.99999999999995737, 216.7545334744432921, 500.8237260975782874 ) ) ;
#9458 = VERTEX_POINT ( 'NONE', #14632 ) ;
#9459 = CARTESIAN_POINT ( 'NONE',  ( -22.99999999999999645, 0.000000000000000000, -36.99999999999999289 ) ) ;
#9460 = DIRECTION ( 'NONE',  ( 0.000000000000000000, -1.000000000000000000, 0.000000000000000000 ) ) ;
#9461 = DIRECTION ( 'NONE',  ( 1.000000000000000000, 0.000000000000000000, 0.000000000000000000 ) ) ;
#9462 = DIRECTION ( 'NONE',  ( -0.000000000000000000, 1.000000000000000000, -0.000000000000000000 ) ) ;
#9463 = DIRECTION ( 'NONE',  ( -0.000000000000000000, -1.000000000000000000, -0.000000000000000000 ) ) ;
#9464 = AXIS2_PLACEMENT_3D ( 'NONE', #9873, #2014, #14100 ) ;
#9465 = DIRECTION ( 'NONE',  ( 0.000000000000000000, 0.000000000000000000, -1.000000000000000000 ) ) ;
#9466 = DIRECTION ( 'NONE',  ( 0.000000000000000000, 0.000000000000000000, -1.000000000000000000 ) ) ;
#9467 = APPLICATION_CONTEXT ( 'automotive_design' ) ;
#9468 = EDGE_CURVE ( 'NONE', #18509, #2620, #94, .T. ) ;
#9469 = CARTESIAN_POINT ( 'NONE',  ( -26.00000000000002132, 10.00000000000000000, -39.99999999999999289 ) ) ;
#9470 = EDGE_CURVE ( 'NONE', #9164, #14816, #17315, .T. ) ;
#9471 = VERTEX_POINT ( 'NONE', #14216 ) ;
#9472 = ORIENTED_EDGE ( 'NONE', *, *, #7862, .T. ) ;
#9473 = PLANE ( 'NONE',  #20210 ) ;
#9474 = ORIENTED_EDGE ( 'NONE', *, *, #173, .F. ) ;
#9475 = EDGE_LOOP ( 'NONE', ( #9989, #14707, #14960, #4147, #11201, #5255, #9202, #19826, #7628, #8346, #19710, #10511, #6185, #5649, #9740, #8350 ) ) ;
#9476 = LINE ( 'NONE', #12692, #12740 ) ;
#9477 =( NAMED_UNIT ( * ) SI_UNIT ( $, .STERADIAN. ) SOLID_ANGLE_UNIT ( ) );
#9478 = AXIS2_PLACEMENT_3D ( 'NONE', #12534, #15956, #12853 ) ;
#9479 = CARTESIAN_POINT ( 'NONE',  ( 34.00000000000002842, 3.000000000000000000, 23.00000000000000355 ) ) ;
#9480 = SURFACE_STYLE_FILL_AREA ( #9274 ) ;
#9481 = CARTESIAN_POINT ( 'NONE',  ( 7.000000000000000000, 0.000000000000000000, 0.000000000000000000 ) ) ;
#9483 = EDGE_CURVE ( 'NONE', #5629, #5220, #18637, .T. ) ;
#9482 = LINE ( 'NONE', #17926, #16591 ) ;
#9484 = CARTESIAN_POINT ( 'NONE',  ( 39.99999999999999289, 10.00000000000000000, 26.00000000000000000 ) ) ;
#9485 = DIRECTION ( 'NONE',  ( -0.000000000000000000, 1.000000000000000000, -0.000000000000000000 ) ) ;
#9486 = PRESENTATION_STYLE_ASSIGNMENT (( #4551 ) ) ;
#9487 = EDGE_CURVE ( 'NONE', #5026, #18463, #6822, .T. ) ;
#9488 = ORIENTED_EDGE ( 'NONE', *, *, #15445, .F. ) ;
#9489 = PRESENTATION_STYLE_ASSIGNMENT (( #18758 ) ) ;
#9490 = DIRECTION ( 'NONE',  ( 0.000000000000000000, 1.000000000000000000, 0.000000000000000000 ) ) ;
#9491 = AXIS2_PLACEMENT_3D ( 'NONE', #3330, #4672, #10857 ) ;
#9492 = ADVANCED_FACE ( 'NONE', ( #14521 ), #7470, .T. ) ;
#9493 = ORIENTED_EDGE ( 'NONE', *, *, #6071, .F. ) ;
#9494 = EDGE_CURVE ( 'NONE', #10221, #1591, #5168, .T. ) ;
#9495 = DIRECTION ( 'NONE',  ( 6.263247009234064878E-17, -0.6381222063396385646, 0.7699350945217602327 ) ) ;
#9496 = VERTEX_POINT ( 'NONE', #11222 ) ;
#9497 = CARTESIAN_POINT ( 'NONE',  ( 111.4893729001366154, 77.72476844875745883, 252.0000000000000000 ) ) ;
#9498 = DIRECTION ( 'NONE',  ( 0.000000000000000000, 0.9187087263927379288, -0.3949357872488051813 ) ) ;
#9499 = ORIENTED_EDGE ( 'NONE', *, *, #14065, .F. ) ;
#9500 = DIRECTION ( 'NONE',  ( 0.000000000000000000, -1.000000000000000000, -7.137148015447440312E-15 ) ) ;
#9501 = CARTESIAN_POINT ( 'NONE',  ( -31.00000000000001776, 10.00000000000000000, 31.00000000000000000 ) ) ;
#9503 = EDGE_CURVE ( 'NONE', #19125, #19958, #9887, .T. ) ;
#9502 = DIRECTION ( 'NONE',  ( -1.000000000000000000, -0.000000000000000000, 0.000000000000000000 ) ) ;
#9504 = AXIS2_PLACEMENT_3D ( 'NONE', #9003, #18372, #18472 ) ;
#9505 = CARTESIAN_POINT ( 'NONE',  ( 0.5200485807784683834, 140.5123536700693876, 500.9436139292040480 ) ) ;
#9506 = CARTESIAN_POINT ( 'NONE',  ( 36.99999999999999289, 0.000000000000000000, 22.99999999999999645 ) ) ;
#9507 = DIRECTION ( 'NONE',  ( 0.000000000000000000, 0.000000000000000000, 1.000000000000000000 ) ) ;
#9508 = LINE ( 'NONE', #15814, #17598 ) ;
#9509 = VERTEX_POINT ( 'NONE', #3198 ) ;
#9510 = SURFACE_STYLE_FILL_AREA ( #1870 ) ;
#9511 = DIRECTION ( 'NONE',  ( 1.000000000000000000, -0.000000000000000000, 0.000000000000000000 ) ) ;
#9512 = APPLICATION_PROTOCOL_DEFINITION ( 'draft international standard', 'automotive_design', 1998, #13053 ) ;
#9513 = EDGE_CURVE ( 'NONE', #14625, #13058, #9476, .T. ) ;
#9514 = CARTESIAN_POINT ( 'NONE',  ( -1.000000000000014655, 152.4824555358010798, 501.3921618609452366 ) ) ;
#9515 = ORIENTED_EDGE ( 'NONE', *, *, #4148, .T. ) ;
#9516 = VECTOR ( 'NONE', #7925, 1000.000000000000000 ) ;
#9517 = ORIENTED_EDGE ( 'NONE', *, *, #17520, .T. ) ;
#9518 = PRESENTATION_LAYER_ASSIGNMENT (  '', '', ( #10169 ) ) ;
#9519 = CIRCLE ( 'NONE', #631, 9.000000000000007105 ) ;
#9520 = ORIENTED_EDGE ( 'NONE', *, *, #13133, .F. ) ;
#9521 = DIRECTION ( 'NONE',  ( -0.000000000000000000, 1.000000000000000000, -0.000000000000000000 ) ) ;
#9522 = VERTEX_POINT ( 'NONE', #11330 ) ;
#9523 = CARTESIAN_POINT ( 'NONE',  ( 0.000000000000000000, 341.0487089519837696, -115.0000000000032969 ) ) ;
#9524 = DIRECTION ( 'NONE',  ( 1.000000000000000000, 9.815121534730718631E-17, 0.000000000000000000 ) ) ;
#9525 = PRESENTATION_STYLE_ASSIGNMENT (( #254 ) ) ;
#9526 = CARTESIAN_POINT ( 'NONE',  ( -80.86158365502321033, 139.7703989349477069, 489.5655098179838092 ) ) ;
#9527 = DIRECTION ( 'NONE',  ( -1.000000000000000000, 0.000000000000000000, 0.000000000000000000 ) ) ;
#9528 =( GEOMETRIC_REPRESENTATION_CONTEXT ( 3 ) GLOBAL_UNCERTAINTY_ASSIGNED_CONTEXT ( ( #3997 ) ) GLOBAL_UNIT_ASSIGNED_CONTEXT ( ( #9155, #15560, #14096 ) ) REPRESENTATION_CONTEXT ( 'NONE', 'WORKASPACE' ) );
#9529 = CARTESIAN_POINT ( 'NONE',  ( 178.4893729001366012, 34.32473510485366575, 0.000000000000000000 ) ) ;
#9530 = EDGE_CURVE ( 'NONE', #16461, #9609, #1153, .T. ) ;
#9531 = ORIENTED_EDGE ( 'NONE', *, *, #20299, .T. ) ;
#9532 = DIRECTION ( 'NONE',  ( -1.000000000000000000, 0.000000000000000000, 0.000000000000000000 ) ) ;
#9533 = DIRECTION ( 'NONE',  ( -0.000000000000000000, 1.000000000000000000, 0.000000000000000000 ) ) ;
#9534 = DIRECTION ( 'NONE',  ( 0.000000000000000000, 0.000000000000000000, -1.000000000000000000 ) ) ;
#9535 = CARTESIAN_POINT ( 'NONE',  ( 35.00000000000000711, 19.00000000000000000, 20.99999999999999289 ) ) ;
#9536 = DIRECTION ( 'NONE',  ( -0.000000000000000000, -0.7791332379872890623, -0.6268583551835633649 ) ) ;
#9537 = LINE ( 'NONE', #6363, #19174 ) ;
#9538 = B_SPLINE_CURVE_WITH_KNOTS ( 'NONE', 3,
 ( #12295, #13839, #16846, #10551, #4362, #11904, #18368, #5710, #20005, #20115, #15190, #12190 ),
 .UNSPECIFIED., .F., .F.,
 ( 4, 2, 2, 2, 2, 4 ),
 ( 0.000000000000000000, 0.0005192799409533858327, 0.001038559881906771665, 0.001557839822860157498, 0.001817479793336867436, 0.002077119763813577592 ),
 .UNSPECIFIED. ) ;
#9539 = SURFACE_SIDE_STYLE ('',( #7899 ) ) ;
#9540 = CYLINDRICAL_SURFACE ( 'NONE', #14478, 3.283624802691453848 ) ;
#9541 = EDGE_CURVE ( 'NONE', #12426, #17668, #3833, .T. ) ;
#9542 = ORIENTED_EDGE ( 'NONE', *, *, #19373, .F. ) ;
#9543 = VECTOR ( 'NONE', #191, 1000.000000000000000 ) ;
#9544 = CIRCLE ( 'NONE', #8252, 10.00000000000000888 ) ;
#9545 = STYLED_ITEM ( 'NONE', ( #3317 ), #6042 ) ;
#9546 = ORIENTED_EDGE ( 'NONE', *, *, #14778, .F. ) ;
#9547 = SURFACE_STYLE_FILL_AREA ( #1697 ) ;
#9548 = CARTESIAN_POINT ( 'NONE',  ( -33.00000000000000000, 8.000000000000000000, -26.00000000000000355 ) ) ;
#9549 = ORIENTED_EDGE ( 'NONE', *, *, #13393, .F. ) ;
#9550 = DIRECTION ( 'NONE',  ( 1.049727191138612163E-16, 0.5150380749100629263, -0.8571673007021070045 ) ) ;
#9551 =( NAMED_UNIT ( * ) SI_UNIT ( $, .STERADIAN. ) SOLID_ANGLE_UNIT ( ) );
#9552 = ORIENTED_EDGE ( 'NONE', *, *, #18691, .T. ) ;
#9553 = DIRECTION ( 'NONE',  ( 8.673617379884027583E-16, 0.000000000000000000, -1.000000000000000000 ) ) ;
#9554 = PRESENTATION_STYLE_ASSIGNMENT (( #15563 ) ) ;
#9555 = DIRECTION ( 'NONE',  ( 1.000000000000000000, -0.000000000000000000, -0.000000000000000000 ) ) ;
#9556 = VECTOR ( 'NONE', #6539, 1000.000000000000000 ) ;
#9557 = CARTESIAN_POINT ( 'NONE',  ( 31.81980515339464333, 8.000000000000000000, -31.81980515339463622 ) ) ;
#9558 = VECTOR ( 'NONE', #15064, 1000.000000000000000 ) ;
#9559 = LINE ( 'NONE', #17395, #14989 ) ;
#9560 = AXIS2_PLACEMENT_3D ( 'NONE', #4043, #18043, #16643 ) ;
#9561 = DIRECTION ( 'NONE',  ( 1.000000000000000000, 0.000000000000000000, 0.000000000000000000 ) ) ;
#9562 = DIRECTION ( 'NONE',  ( 1.000000000000000000, -0.000000000000000000, 0.000000000000000000 ) ) ;
#9563 = EDGE_CURVE ( 'NONE', #10819, #6194, #19603, .T. ) ;
#9564 = VERTEX_POINT ( 'NONE', #19549 ) ;
#9565 = EDGE_LOOP ( 'NONE', ( #1587, #6841, #5882, #15529 ) ) ;
#9566 = VERTEX_POINT ( 'NONE', #13590 ) ;
#9567 = ORIENTED_EDGE ( 'NONE', *, *, #4514, .F. ) ;
#9568 = DIRECTION ( 'NONE',  ( 1.000000000000000000, 0.000000000000000000, 0.000000000000000000 ) ) ;
#9569 = VECTOR ( 'NONE', #19264, 1000.000000000000000 ) ;
#9570 = VECTOR ( 'NONE', #16920, 1000.000000000000000 ) ;
#9571 = CARTESIAN_POINT ( 'NONE',  ( 503.8334540492693918, 167.8734308960555950, 0.000000000000000000 ) ) ;
#9572 = DIRECTION ( 'NONE',  ( 1.000000000000000000, 0.000000000000000000, 0.000000000000000000 ) ) ;
#9573 = CYLINDRICAL_SURFACE ( 'NONE', #14466, 5.000000000000000888 ) ;
#9574 = DIRECTION ( 'NONE',  ( -0.000000000000000000, -1.000000000000000000, 0.000000000000000000 ) ) ;
#9575 = PRODUCT ( 'Part15', 'Part15', '', ( #18475 ) ) ;
#9576 = ORIENTED_EDGE ( 'NONE', *, *, #16790, .T. ) ;
#9577 = LINE ( 'NONE', #11133, #8812 ) ;
#9578 = ADVANCED_FACE ( 'NONE', ( #13203 ), #8456, .F. ) ;
#9579 = CARTESIAN_POINT ( 'NONE',  ( -26.00000000000002132, 0.000000000000000000, -31.00000000000003553 ) ) ;
#9580 = ORIENTED_EDGE ( 'NONE', *, *, #16182, .F. ) ;
#9581 = DIRECTION ( 'NONE',  ( 0.000000000000000000, -0.7071067811865504593, 0.7071067811865445751 ) ) ;
#9582 = CYLINDRICAL_SURFACE ( 'NONE', #5748, 10.00000000000000888 ) ;
#9583 = VECTOR ( 'NONE', #19006, 1000.000000000000000 ) ;
#9584 = CIRCLE ( 'NONE', #3691, 5.000000000000000888 ) ;
#9585 = EDGE_CURVE ( 'NONE', #3302, #1869, #3708, .T. ) ;
#9586 = VERTEX_POINT ( 'NONE', #4123 ) ;
#9587 = FILL_AREA_STYLE_COLOUR ( '', #12542 ) ;
#9588 = PRODUCT_RELATED_PRODUCT_CATEGORY ( 'part', '', ( #17323 ) ) ;
#9589 = ORIENTED_EDGE ( 'NONE', *, *, #17584, .F. ) ;
#9590 =( GEOMETRIC_REPRESENTATION_CONTEXT ( 3 ) GLOBAL_UNCERTAINTY_ASSIGNED_CONTEXT ( ( #20190 ) ) GLOBAL_UNIT_ASSIGNED_CONTEXT ( ( #864, #19813, #7080 ) ) REPRESENTATION_CONTEXT ( 'NONE', 'WORKASPACE' ) );
#9591 =( NAMED_UNIT ( * ) PLANE_ANGLE_UNIT ( ) SI_UNIT ( $, .RADIAN. ) );
#9592 = EDGE_LOOP ( 'NONE', ( #10568, #18362, #10997, #1861 ) ) ;
#9593 = CARTESIAN_POINT ( 'NONE',  ( -82.18192946989275072, 216.7545334744432921, 499.8237260975782306 ) ) ;
#9594 = STYLED_ITEM ( 'NONE', ( #3891 ), #8135 ) ;
#9595 = ADVANCED_FACE ( 'NONE', ( #16705 ), #11749, .T. ) ;
#9596 = DIRECTION ( 'NONE',  ( 0.000000000000000000, 0.000000000000000000, -1.000000000000000000 ) ) ;
#9597 = DIRECTION ( 'NONE',  ( 1.000000000000000000, 0.000000000000000000, 0.000000000000000000 ) ) ;
#9598 = LINE ( 'NONE', #4786, #4955 ) ;
#9599 = FACE_OUTER_BOUND ( 'NONE', #3086, .T. ) ;
#9600 = VECTOR ( 'NONE', #2736, 1000.000000000000000 ) ;
#9601 = EDGE_LOOP ( 'NONE', ( #19496, #14017, #8420, #2946 ) ) ;
#9602 = EDGE_CURVE ( 'NONE', #4977, #10759, #17972, .T. ) ;
#9603 = DIRECTION ( 'NONE',  ( 1.000000000000000000, 0.000000000000000000, 0.000000000000000000 ) ) ;
#9604 = FACE_OUTER_BOUND ( 'NONE', #8196, .T. ) ;
#9605 = ITEM_DEFINED_TRANSFORMATION ( 'NONE', 'NONE', #6727,  #2741 ) ;
#9606 = EDGE_LOOP ( 'NONE', ( #1879, #13427, #18175, #7327, #13152 ) ) ;
#9607 = ORIENTED_EDGE ( 'NONE', *, *, #13216, .F. ) ;
#9608 = SURFACE_STYLE_USAGE ( .BOTH. , #15731 ) ;
#9609 = VERTEX_POINT ( 'NONE', #5356 ) ;
#9610 = VECTOR ( 'NONE', #12535, 1000.000000000000000 ) ;
#9611 = ORIENTED_EDGE ( 'NONE', *, *, #17584, .T. ) ;
#9612 = EDGE_CURVE ( 'NONE', #12998, #886, #9100, .T. ) ;
#9613 = COLOUR_RGB ( '', 0.72549020, 0.75294118, 0.79215686) ;
#9614 = ORIENTED_EDGE ( 'NONE', *, *, #19563, .T. ) ;
#9615 = CARTESIAN_POINT ( 'NONE',  ( -64.99999999999995737, 317.7545334744432353, 495.1946179577816451 ) ) ;
#9616 = DIRECTION ( 'NONE',  ( 0.000000000000000000, 0.000000000000000000, 1.000000000000000000 ) ) ;
#9617 = CARTESIAN_POINT ( 'NONE',  ( 35.00000000000000711, 8.000000000000000000, 20.99999999999999289 ) ) ;
#9618 = EDGE_CURVE ( 'NONE', #14706, #368, #4896, .T. ) ;
#9619 = VERTEX_POINT ( 'NONE', #10904 ) ;
#9620 = CIRCLE ( 'NONE', #10614, 10.00000000000000888 ) ;
#9621 = CYLINDRICAL_SURFACE ( 'NONE', #6068, 2.999999999999995559 ) ;
#9622 = FILL_AREA_STYLE_COLOUR ( '', #17801 ) ;
#9623 = ORIENTED_EDGE ( 'NONE', *, *, #4733, .F. ) ;
#9624 = ADVANCED_FACE ( 'NONE', ( #12452, #19953, #12137, #18319, #12351 ), #9352, .F. ) ;
#9625 = CARTESIAN_POINT ( 'NONE',  ( 31.00000000000000000, 19.00000000000000000, -31.00000000000000355 ) ) ;
#9626 = DIRECTION ( 'NONE',  ( 1.000000000000000000, -0.000000000000000000, 0.000000000000000000 ) ) ;
#9627 = CARTESIAN_POINT ( 'NONE',  ( 78.48937290013661539, 80.91625508013694912, -140.0000000000001137 ) ) ;
#9628 = VECTOR ( 'NONE', #6054, 1000.000000000000000 ) ;
#9629 = AXIS2_PLACEMENT_3D ( 'NONE', #11833, #9035, #1067 ) ;
#9630 = LINE ( 'NONE', #15844, #5689 ) ;
#9631 = EDGE_CURVE ( 'NONE', #3967, #6864, #20049, .T. ) ;
#9632 = DIRECTION ( 'NONE',  ( -1.000000000000000000, -0.000000000000000000, -0.000000000000000000 ) ) ;
#9633 = CARTESIAN_POINT ( 'NONE',  ( -2.383085342081997293, 39.16728066132458963, 9.196931476227280911 ) ) ;
#9634 = STYLED_ITEM ( 'NONE', ( #939 ), #8501 ) ;
#9635 = VERTEX_POINT ( 'NONE', #6067 ) ;
#9636 = ADVANCED_FACE ( 'NONE', ( #7814 ), #14092, .F. ) ;
#9637 = CARTESIAN_POINT ( 'NONE',  ( 37.00000000000000000, 0.000000000000000000, 23.00000000000001066 ) ) ;
#9638 = DIRECTION ( 'NONE',  ( -0.000000000000000000, -1.000000000000000000, -0.000000000000000000 ) ) ;
#9639 = LINE ( 'NONE', #11188, #14931 ) ;
#9640 = SHAPE_REPRESENTATION_RELATIONSHIP ( 'NONE' , 'NONE' ,  #10923, #7901 ) ;
#9641 = FACE_OUTER_BOUND ( 'NONE', #15719, .T. ) ;
#9642 = CARTESIAN_POINT ( 'NONE',  ( 34.99999999999997868, 0.000000000000000000, 40.00000000000000711 ) ) ;
#9643 = STYLED_ITEM ( 'NONE', ( #16798 ), #170 ) ;
#9644 = CARTESIAN_POINT ( 'NONE',  ( 31.00000000000001421, 6.000000000000000000, 22.99999999999999645 ) ) ;
#9645 = ORIENTED_EDGE ( 'NONE', *, *, #5353, .T. ) ;
#9646 = EDGE_CURVE ( 'NONE', #2022, #18268, #1082, .T. ) ;
#9647 = ORIENTED_EDGE ( 'NONE', *, *, #3577, .T. ) ;
#9648 = LINE ( 'NONE', #15973, #15994 ) ;
#9649 = VECTOR ( 'NONE', #16312, 1000.000000000000000 ) ;
#9650 = ORIENTED_EDGE ( 'NONE', *, *, #15713, .F. ) ;
#9651 = DIRECTION ( 'NONE',  ( 1.000000000000000000, -0.000000000000000000, -0.000000000000000000 ) ) ;
#9652 = CARTESIAN_POINT ( 'NONE',  ( -80.12128812903169717, 140.0129565146422124, 501.2795744101462674 ) ) ;
#9653 = ORIENTED_EDGE ( 'NONE', *, *, #18375, .T. ) ;
#9654 = VECTOR ( 'NONE', #13809, 1000.000000000000000 ) ;
#9655 = CIRCLE ( 'NONE', #16581, 9.000000000000007105 ) ;
#9656 = ORIENTED_EDGE ( 'NONE', *, *, #6997, .T. ) ;
#9657 = ADVANCED_FACE ( 'NONE', ( #16894 ), #9053, .F. ) ;
#9658 = LINE ( 'NONE', #1706, #318 ) ;
#9659 = CARTESIAN_POINT ( 'NONE',  ( 34.00000000000002842, -20.00000000000000000, 26.00000000000000355 ) ) ;
#9660 = ADVANCED_FACE ( 'NONE', ( #16998 ), #2853, .T. ) ;
#9661 = DIRECTION ( 'NONE',  ( -0.000000000000000000, 1.000000000000000000, 0.000000000000000000 ) ) ;
#9662 = LINE ( 'NONE', #8137, #11454 ) ;
#9663 = CIRCLE ( 'NONE', #17557, 14.27500000000000036 ) ;
#9664 = VECTOR ( 'NONE', #15753, 1000.000000000000000 ) ;
#9665 = ADVANCED_FACE ( 'NONE', ( #7603 ), #1242, .T. ) ;
#9666 =( NAMED_UNIT ( * ) SI_UNIT ( $, .STERADIAN. ) SOLID_ANGLE_UNIT ( ) );
#9667 = DIRECTION ( 'NONE',  ( -1.000000000000000000, -0.000000000000000000, -0.000000000000000000 ) ) ;
#9668 = STYLED_ITEM ( 'NONE', ( #1278 ), #7987 ) ;
#9669 = CARTESIAN_POINT ( 'NONE',  ( 0.000000000000000000, 66.00000000000000000, 1.799999999999999600 ) ) ;
#9670 = CARTESIAN_POINT ( 'NONE',  ( 0.000000000000000000, 316.7545334744432353, 495.1946179577816451 ) ) ;
#9671 = CARTESIAN_POINT ( 'NONE',  ( 503.8334540492693918, 242.8734308960556234, 0.000000000000000000 ) ) ;
#9672 = CARTESIAN_POINT ( 'NONE',  ( 423.8334540492694487, 191.8198460455371333, 168.2339398819845826 ) ) ;
#9673 = ORIENTED_EDGE ( 'NONE', *, *, #14322, .F. ) ;
#9674 = VECTOR ( 'NONE', #18771, 1000.000000000000000 ) ;
#9675 = VECTOR ( 'NONE', #8042, 1000.000000000000000 ) ;
#9676 = EDGE_LOOP ( 'NONE', ( #15033, #18476, #11282, #17689 ) ) ;
#9677 = VERTEX_POINT ( 'NONE', #5031 ) ;
#9678 = DIRECTION ( 'NONE',  ( 1.000000000000000000, -0.000000000000000000, -0.000000000000000000 ) ) ;
#9679 = ORIENTED_EDGE ( 'NONE', *, *, #2040, .F. ) ;
#9680 = VERTEX_POINT ( 'NONE', #11415 ) ;
#9681 = CIRCLE ( 'NONE', #9033, 3.883636366625808911 ) ;
#9682 = COLOUR_RGB ( '', 0.72549020, 0.75294118, 0.79215686) ;
#9683 = ORIENTED_EDGE ( 'NONE', *, *, #3811, .T. ) ;
#9684 = DIRECTION ( 'NONE',  ( 0.000000000000000000, 0.000000000000000000, 1.000000000000000000 ) ) ;
#9685 = DIRECTION ( 'NONE',  ( 1.000000000000000000, -0.000000000000000000, -0.000000000000000000 ) ) ;
#9686 = SURFACE_STYLE_FILL_AREA ( #3406 ) ;
#9687 = LINE ( 'NONE', #6502, #14131 ) ;
#9688 = DIRECTION ( 'NONE',  ( 0.000000000000000000, 0.000000000000000000, -1.000000000000000000 ) ) ;
#9689 =( GEOMETRIC_REPRESENTATION_CONTEXT ( 3 ) GLOBAL_UNCERTAINTY_ASSIGNED_CONTEXT ( ( #5818 ) ) GLOBAL_UNIT_ASSIGNED_CONTEXT ( ( #7450, #18134, #18248 ) ) REPRESENTATION_CONTEXT ( 'NONE', 'WORKASPACE' ) );
#9690 = EDGE_LOOP ( 'NONE', ( #9404, #16093, #2506, #7659 ) ) ;
#9691 = EDGE_CURVE ( 'NONE', #18923, #159, #14397, .T. ) ;
#9692 = CARTESIAN_POINT ( 'NONE',  ( 0.9699764831012678279, 62.84572122215210754, 9.452135968713493597 ) ) ;
#9693 = AXIS2_PLACEMENT_3D ( 'NONE', #8893, #15183, #13638 ) ;
#9694 = CARTESIAN_POINT ( 'NONE',  ( 153.4893729001366580, 80.91625508013694912, -140.0000000000001137 ) ) ;
#9695 = FILL_AREA_STYLE ('',( #3413 ) ) ;
#9696 = CARTESIAN_POINT ( 'NONE',  ( 0.000000000000000000, 376.0487089519831443, -75.00000000000331113 ) ) ;
#9697 = ORIENTED_EDGE ( 'NONE', *, *, #8485, .F. ) ;
#9698 = CARTESIAN_POINT ( 'NONE',  ( -78.99999999999995737, 141.6406393683236331, 501.8237260975782874 ) ) ;
#9699 = AXIS2_PLACEMENT_3D ( 'NONE', #20324, #10855, #5914 ) ;
#9700 = VECTOR ( 'NONE', #12707, 1000.000000000000000 ) ;
#9701 = LINE ( 'NONE', #10006, #19873 ) ;
#9702 = PRESENTATION_LAYER_ASSIGNMENT (  '', '', ( #2127 ) ) ;
#9703 = CIRCLE ( 'NONE', #2114, 10.00000000000000888 ) ;
#9704 = ORIENTED_EDGE ( 'NONE', *, *, #12398, .T. ) ;
#9705 = AXIS2_PLACEMENT_3D ( 'NONE', #18336, #10204, #2673 ) ;
#9706 = ORIENTED_EDGE ( 'NONE', *, *, #8989, .T. ) ;
#9707 = VECTOR ( 'NONE', #5338, 1000.000000000000000 ) ;
#9708 = FACE_OUTER_BOUND ( 'NONE', #6010, .T. ) ;
#9709 = ORIENTED_EDGE ( 'NONE', *, *, #18922, .F. ) ;
#9710 = AXIS2_PLACEMENT_3D ( 'NONE', #7344, #5293, #10327 ) ;
#9711 = CARTESIAN_POINT ( 'NONE',  ( 26.00000000000000355, 11.00000000000000000, -40.00000000000000711 ) ) ;
#9712 = MECHANICAL_DESIGN_GEOMETRIC_PRESENTATION_REPRESENTATION (  '', ( #16640 ), #822 ) ;
#9713 = ORIENTED_EDGE ( 'NONE', *, *, #3415, .T. ) ;
#9714 =( BOUNDED_CURVE ( )  B_SPLINE_CURVE ( 3, ( #3232, #17247, #10760, #13954 ),
 .UNSPECIFIED., .F., .T. ) 
 B_SPLINE_CURVE_WITH_KNOTS ( ( 4, 4 ),
 ( 4.712388980384689674, 6.283185307179586232 ),
 .UNSPECIFIED. ) 
 CURVE ( )  GEOMETRIC_REPRESENTATION_ITEM ( )  RATIONAL_B_SPLINE_CURVE ( ( 1.000000000000000000, 0.8047378541243649375, 0.8047378541243649375, 1.000000000000000000 ) ) 
 REPRESENTATION_ITEM ( '' )  );
#9715 = CARTESIAN_POINT ( 'NONE',  ( -64.99999999999995737, 317.7545334744432353, 495.1946179577816451 ) ) ;
#9716 = CARTESIAN_POINT ( 'NONE',  ( 4.163799117101000559E-15, 0.000000000000000000, 34.00000000000000000 ) ) ;
#9717 = COLOUR_RGB ( '', 0.40784314, 0.44705882, 0.49803922) ;
#9718 = EDGE_CURVE ( 'NONE', #2774, #9164, #13086, .T. ) ;
#9719 = FILL_AREA_STYLE ('',( #3434 ) ) ;
#9720 = CARTESIAN_POINT ( 'NONE',  ( 30.99999999999999645, 68.00000000000000000, 26.00000000000001066 ) ) ;
#9721 = LINE ( 'NONE', #14357, #1881 ) ;
#9722 = VECTOR ( 'NONE', #12718, 1000.000000000000000 ) ;
#9723 = DIRECTION ( 'NONE',  ( 1.000000000000000000, -0.000000000000000000, 0.000000000000000000 ) ) ;
#9724 = CYLINDRICAL_SURFACE ( 'NONE', #13829, 3.000000000000002665 ) ;
#9725 = CARTESIAN_POINT ( 'NONE',  ( 31.81980515339464333, 0.000000000000000000, -35.11980515339463693 ) ) ;
#9726 = ORIENTED_EDGE ( 'NONE', *, *, #5335, .T. ) ;
#9727 = CARTESIAN_POINT ( 'NONE',  ( 31.81980515339464333, 11.00000000000000000, -28.51980515339463906 ) ) ;
#9728 = LINE ( 'NONE', #19082, #18110 ) ;
#9729 = PLANE ( 'NONE',  #3435 ) ;
#9730 = VECTOR ( 'NONE', #12622, 1000.000000000000000 ) ;
#9731 = CARTESIAN_POINT ( 'NONE',  ( 17.99999999999998579, 6.000000000000000000, -36.99999999999999289 ) ) ;
#9732 = ORIENTED_EDGE ( 'NONE', *, *, #1513, .T. ) ;
#9733 = ORIENTED_EDGE ( 'NONE', *, *, #15686, .T. ) ;
#9734 = VERTEX_POINT ( 'NONE', #19247 ) ;
#9735 = EDGE_CURVE ( 'NONE', #1869, #5907, #10420, .T. ) ;
#9736 = EDGE_LOOP ( 'NONE', ( #17146, #18032 ) ) ;
#9737 = CONICAL_SURFACE ( 'NONE', #19924, 12.32407335584850117, 0.8899833664651138898 ) ;
#9738 = CARTESIAN_POINT ( 'NONE',  ( -41.50085094405407915, 175.4489062796178871, 510.3921618609452935 ) ) ;
#9739 = SURFACE_STYLE_USAGE ( .BOTH. , #18129 ) ;
#9740 = ORIENTED_EDGE ( 'NONE', *, *, #9904, .T. ) ;
#9741 = CARTESIAN_POINT ( 'NONE',  ( 0.1778267103069386679, 139.8640615783817793, 489.1502978112980600 ) ) ;
#9742 = VECTOR ( 'NONE', #16248, 1000.000000000000000 ) ;
#9743 = ORIENTED_EDGE ( 'NONE', *, *, #12487, .T. ) ;
#9744 = DIRECTION ( 'NONE',  ( 1.000000000000000000, 5.889072920838430686E-16, -0.000000000000000000 ) ) ;
#9745 = PLANE ( 'NONE',  #8639 ) ;
#9746 = DIRECTION ( 'NONE',  ( -0.000000000000000000, -0.000000000000000000, -1.000000000000000000 ) ) ;
#9747 = FACE_OUTER_BOUND ( 'NONE', #10608, .T. ) ;
#9748 = SURFACE_STYLE_USAGE ( .BOTH. , #1480 ) ;
#9749 = ADVANCED_FACE ( 'NONE', ( #11299 ), #272, .F. ) ;
#9750 = CARTESIAN_POINT ( 'NONE',  ( -2.901926423773061536, 40.21397019809104023, 9.046021540735431188 ) ) ;
#9751 = VERTEX_POINT ( 'NONE', #1904 ) ;
#9752 = DIRECTION ( 'NONE',  ( 0.000000000000000000, 0.000000000000000000, -1.000000000000000000 ) ) ;
#9753 = CARTESIAN_POINT ( 'NONE',  ( 109.4893729001365870, 209.7811923590224978, 348.0151256184570343 ) ) ;
#9754 = CARTESIAN_POINT ( 'NONE',  ( 111.4893729001366012, 211.0574367717017594, 346.4752554294135507 ) ) ;
#9755 = LINE ( 'NONE', #1896, #4401 ) ;
#9756 = CIRCLE ( 'NONE', #4489, 13.29999999999999893 ) ;
#9757 = VERTEX_POINT ( 'NONE', #367 ) ;
#9758 = EDGE_CURVE ( 'NONE', #7437, #1029, #6683, .T. ) ;
#9759 = CYLINDRICAL_SURFACE ( 'NONE', #20043, 10.00000000000000888 ) ;
#9760 = VERTEX_POINT ( 'NONE', #10262 ) ;
#9761 = AXIS2_PLACEMENT_3D ( 'NONE', #14329, #12791, #392 ) ;
#9762 = EDGE_CURVE ( 'NONE', #9383, #7830, #3981, .T. ) ;
#9763 = EDGE_LOOP ( 'NONE', ( #12095, #2170, #17883, #9472 ) ) ;
#9764 = EDGE_CURVE ( 'NONE', #13515, #2973, #539, .T. ) ;
#9765 = PRODUCT_DEFINITION_SHAPE ( 'NONE', 'NONE',  #20378 ) ;
#9766 = ORIENTED_EDGE ( 'NONE', *, *, #16475, .F. ) ;
#9767 = DIRECTION ( 'NONE',  ( 0.000000000000000000, 0.000000000000000000, 1.000000000000000000 ) ) ;
#9768 = EDGE_CURVE ( 'NONE', #140, #5163, #15366, .T. ) ;
#9769 = DIRECTION ( 'NONE',  ( 0.000000000000000000, -1.000000000000000000, 0.000000000000000000 ) ) ;
#9770 = ORIENTED_EDGE ( 'NONE', *, *, #2185, .F. ) ;
#9771 = DIRECTION ( 'NONE',  ( 0.000000000000000000, 0.000000000000000000, -1.000000000000000000 ) ) ;
#9772 =( NAMED_UNIT ( * ) SI_UNIT ( $, .STERADIAN. ) SOLID_ANGLE_UNIT ( ) );
#9773 = ORIENTED_EDGE ( 'NONE', *, *, #9948, .F. ) ;
#9774 = CARTESIAN_POINT ( 'NONE',  ( 40.00000000000000711, 0.000000000000000000, 34.99999999999997868 ) ) ;
#9775 = VECTOR ( 'NONE', #15421, 1000.000000000000000 ) ;
#9776 =( NAMED_UNIT ( * ) PLANE_ANGLE_UNIT ( ) SI_UNIT ( $, .RADIAN. ) );
#9777 = EDGE_CURVE ( 'NONE', #9081, #17030, #17993, .T. ) ;
#9778 = DIRECTION ( 'NONE',  ( 1.000000000000000000, 0.000000000000000000, 0.000000000000000000 ) ) ;
#9779 = DIRECTION ( 'NONE',  ( -6.123031769111888756E-17, 1.000000000000000000, 3.749151804555346336E-33 ) ) ;
#9780 = PRESENTATION_STYLE_ASSIGNMENT (( #13285 ) ) ;
#9781 = CARTESIAN_POINT ( 'NONE',  ( 5.162501635565829972, -12.32407335584850117, 1.509263698769704680E-15 ) ) ;
#9782 = LINE ( 'NONE', #5160, #12140 ) ;
#9783 = DIRECTION ( 'NONE',  ( -0.000000000000000000, 1.000000000000000000, -0.000000000000000000 ) ) ;
#9784 = DIRECTION ( 'NONE',  ( 0.000000000000000000, 1.000000000000000000, 0.000000000000000000 ) ) ;
#9785 = EDGE_LOOP ( 'NONE', ( #7909, #16432, #18187, #2282 ) ) ;
#9786 = EDGE_CURVE ( 'NONE', #6397, #2527, #3528, .T. ) ;
#9787 = ORIENTED_EDGE ( 'NONE', *, *, #767, .F. ) ;
#9788 = EDGE_CURVE ( 'NONE', #12515, #14600, #673, .T. ) ;
#9789 = ORIENTED_EDGE ( 'NONE', *, *, #8136, .F. ) ;
#9790 = UNCERTAINTY_MEASURE_WITH_UNIT (LENGTH_MEASURE( 1.000000000000000082E-05 ), #12118, 'distance_accuracy_value', 'NONE');
#9791 = ORIENTED_EDGE ( 'NONE', *, *, #10396, .T. ) ;
#9792 = ORIENTED_EDGE ( 'NONE', *, *, #1249, .T. ) ;
#9793 = DIRECTION ( 'NONE',  ( -0.000000000000000000, 1.000000000000000000, -0.000000000000000000 ) ) ;
#9794 = CARTESIAN_POINT ( 'NONE',  ( 53.48937290013660117, 77.72476844875745883, 252.0000000000000000 ) ) ;
#9795 = FILL_AREA_STYLE ('',( #19155 ) ) ;
#9796 = DIRECTION ( 'NONE',  ( -0.000000000000000000, -1.000000000000000000, -0.000000000000000000 ) ) ;
#9797 = DIRECTION ( 'NONE',  ( 0.000000000000000000, 1.000000000000000000, 0.000000000000000000 ) ) ;
#9798 = CARTESIAN_POINT ( 'NONE',  ( 1.831162533324887542, 62.38426314815912832, 9.323294315095143503 ) ) ;
#9799 =( GEOMETRIC_REPRESENTATION_CONTEXT ( 3 ) GLOBAL_UNCERTAINTY_ASSIGNED_CONTEXT ( ( #14686 ) ) GLOBAL_UNIT_ASSIGNED_CONTEXT ( ( #10498, #17089, #10916 ) ) REPRESENTATION_CONTEXT ( 'NONE', 'WORKASPACE' ) );
#9800 = DIRECTION ( 'NONE',  ( 1.000000000000000000, -0.000000000000000000, -0.000000000000000000 ) ) ;
#9801 = LINE ( 'NONE', #9694, #785 ) ;
#9802 =( NAMED_UNIT ( * ) PLANE_ANGLE_UNIT ( ) SI_UNIT ( $, .RADIAN. ) );
#9803 = CYLINDRICAL_SURFACE ( 'NONE', #1057, 3.000000000000002665 ) ;
#9804 = EDGE_CURVE ( 'NONE', #9122, #6311, #9106, .T. ) ;
#9805 = CARTESIAN_POINT ( 'NONE',  ( 32.99999999999998579, 10.00000000000000000, 21.99999999999999645 ) ) ;
#9806 = CARTESIAN_POINT ( 'NONE',  ( -31.81980515339462912, 8.000000000000000000, 35.11980515339465825 ) ) ;
#9807 = EDGE_CURVE ( 'NONE', #6976, #9496, #14798, .T. ) ;
#9808 = EDGE_CURVE ( 'NONE', #9677, #19312, #8513, .T. ) ;
#9809 = AXIS2_PLACEMENT_3D ( 'NONE', #329, #6326, #12604 ) ;
#9810 = EDGE_LOOP ( 'NONE', ( #16076, #16849, #16419, #14681 ) ) ;
#9811 = VECTOR ( 'NONE', #1168, 1000.000000000000000 ) ;
#9812 = DIRECTION ( 'NONE',  ( -1.000000000000000000, -9.815121534730717399E-17, 0.000000000000000000 ) ) ;
#9813 = EDGE_LOOP ( 'NONE', ( #2337, #5410, #16281, #2146 ) ) ;
#9814 = PRESENTATION_STYLE_ASSIGNMENT (( #3426 ) ) ;
#9815 = EDGE_LOOP ( 'NONE', ( #19511, #16194 ) ) ;
#9816 = CARTESIAN_POINT ( 'NONE',  ( 40.00000000000000711, 11.00000000000000000, 25.99999999999999645 ) ) ;
#9817 = FACE_OUTER_BOUND ( 'NONE', #6775, .T. ) ;
#9818 = VERTEX_POINT ( 'NONE', #19518 ) ;
#9819 = FACE_BOUND ( 'NONE', #5733, .T. ) ;
#9820 = CARTESIAN_POINT ( 'NONE',  ( 22.99999999999998224, 6.000000000000000000, -31.00000000000003197 ) ) ;
#9821 = DIRECTION ( 'NONE',  ( 1.000000000000000000, 5.889072920838430686E-16, -0.000000000000000000 ) ) ;
#9822 = LINE ( 'NONE', #1866, #3650 ) ;
#9823 = FACE_OUTER_BOUND ( 'NONE', #9676, .T. ) ;
#9824 = LINE ( 'NONE', #2068, #20217 ) ;
#9825 = AXIS2_PLACEMENT_3D ( 'NONE', #3255, #1683, #358 ) ;
#9826 = ORIENTED_EDGE ( 'NONE', *, *, #15420, .F. ) ;
#9827 = FILL_AREA_STYLE_COLOUR ( '', #5555 ) ;
#9828 = DIRECTION ( 'NONE',  ( 1.000000000000000000, 0.000000000000000000, 0.000000000000000000 ) ) ;
#9829 = DIRECTION ( 'NONE',  ( 0.000000000000000000, 0.000000000000000000, -1.000000000000000000 ) ) ;
#9830 = VERTEX_POINT ( 'NONE', #14907 ) ;
#9831 = DIRECTION ( 'NONE',  ( 0.000000000000000000, 0.000000000000000000, -1.000000000000000000 ) ) ;
#9832 = VERTEX_POINT ( 'NONE', #5235 ) ;
#9833 = EDGE_CURVE ( 'NONE', #19270, #716, #770, .T. ) ;
#9834 = ORIENTED_EDGE ( 'NONE', *, *, #12887, .T. ) ;
#9835 = ORIENTED_EDGE ( 'NONE', *, *, #10108, .F. ) ;
#9836 = CARTESIAN_POINT ( 'NONE',  ( -41.50085094405407915, 159.0821755739672483, 505.3921618609452935 ) ) ;
#9837 =( GEOMETRIC_REPRESENTATION_CONTEXT ( 3 ) GLOBAL_UNCERTAINTY_ASSIGNED_CONTEXT ( ( #449 ) ) GLOBAL_UNIT_ASSIGNED_CONTEXT ( ( #13048, #437, #3645 ) ) REPRESENTATION_CONTEXT ( 'NONE', 'WORKASPACE' ) );
#9838 = ORIENTED_EDGE ( 'NONE', *, *, #11980, .F. ) ;
#9839 = PRESENTATION_STYLE_ASSIGNMENT (( #17866 ) ) ;
#9840 = CARTESIAN_POINT ( 'NONE',  ( 423.8334540492694487, 191.8198460455371333, 34.99421986894476788 ) ) ;
#9841 = DIRECTION ( 'NONE',  ( 1.000000000000000000, 0.000000000000000000, 0.000000000000000000 ) ) ;
#9842 = LINE ( 'NONE', #16156, #11945 ) ;
#9843 = DIRECTION ( 'NONE',  ( 0.000000000000000000, -1.000000000000000000, -1.632680918566406793E-16 ) ) ;
#9844 = CARTESIAN_POINT ( 'NONE',  ( -41.50085094405408626, 209.4098724938429541, 505.3921618609452935 ) ) ;
#9845 = SURFACE_SIDE_STYLE ('',( #563 ) ) ;
#9846 = ORIENTED_EDGE ( 'NONE', *, *, #7640, .T. ) ;
#9847 = CARTESIAN_POINT ( 'NONE',  ( 1.181929469892510243, 139.7703989349544145, 490.5655098179848892 ) ) ;
#9848 = EDGE_CURVE ( 'NONE', #2620, #16062, #6165, .T. ) ;
#9849 = FILL_AREA_STYLE ('',( #9953 ) ) ;
#9850 = PRESENTATION_STYLE_ASSIGNMENT (( #19615 ) ) ;
#9851 = SHAPE_REPRESENTATION_RELATIONSHIP ( 'NONE' , 'NONE' ,  #11716, #13561 ) ;
#9852 = PRESENTATION_LAYER_ASSIGNMENT (  '', '', ( #18723 ) ) ;
#9853 = CARTESIAN_POINT ( 'NONE',  ( -31.00000000000000000, 19.00000000000000000, -31.00000000000000000 ) ) ;
#9854 = CARTESIAN_POINT ( 'NONE',  ( 0.000000000000000000, 50.00000000000000000, -36.50000000000000000 ) ) ;
#9855 = ORIENTED_EDGE ( 'NONE', *, *, #6105, .F. ) ;
#9856 = ORIENTED_EDGE ( 'NONE', *, *, #12566, .F. ) ;
#9857 = EDGE_CURVE ( 'NONE', #2216, #469, #11608, .T. ) ;
#9858 = ORIENTED_EDGE ( 'NONE', *, *, #62, .F. ) ;
#9859 =( NAMED_UNIT ( * ) PLANE_ANGLE_UNIT ( ) SI_UNIT ( $, .RADIAN. ) );
#9860 = APPLICATION_CONTEXT ( 'automotive_design' ) ;
#9861 = CARTESIAN_POINT ( 'NONE',  ( 2.799999999999999822, 0.000000000000000000, 0.000000000000000000 ) ) ;
#9862 = VERTEX_POINT ( 'NONE', #19623 ) ;
#9863 = COLOUR_RGB ( '', 0.40784314, 0.44705882, 0.49803922) ;
#9864 = CARTESIAN_POINT ( 'NONE',  ( 463.8334540492693350, 191.8198460455371333, 34.99421986894476788 ) ) ;
#9865 = PRESENTATION_LAYER_ASSIGNMENT (  '', '', ( #8534 ) ) ;
#9866 = LINE ( 'NONE', #5146, #12587 ) ;
#9867 = EDGE_CURVE ( 'NONE', #8369, #7486, #7092, .T. ) ;
#9868 = VERTEX_POINT ( 'NONE', #17789 ) ;
#9869 = DIRECTION ( 'NONE',  ( -0.000000000000000000, -0.000000000000000000, 1.000000000000000000 ) ) ;
#9870 = DIRECTION ( 'NONE',  ( 1.000000000000000000, 0.000000000000000000, -0.000000000000000000 ) ) ;
#9871 = SURFACE_SIDE_STYLE ('',( #75 ) ) ;
#9872 = CARTESIAN_POINT ( 'NONE',  ( -1.000000000000000888, 138.7545334744432637, 477.3411705753777596 ) ) ;
#9873 = CARTESIAN_POINT ( 'NONE',  ( -58.16843972078500258, 319.7545334744432353, 485.1700099148404206 ) ) ;
#9874 = ADVANCED_BREP_SHAPE_REPRESENTATION ( '', ( #15136, #2741 ), #3403 ) ;
#9875 =( NAMED_UNIT ( * ) PLANE_ANGLE_UNIT ( ) SI_UNIT ( $, .RADIAN. ) );
#9876 = CARTESIAN_POINT ( 'NONE',  ( 0.000000000000000000, 10.00000000000000000, 0.000000000000000000 ) ) ;
#9877 = LINE ( 'NONE', #9670, #19688 ) ;
#9878 = DIRECTION ( 'NONE',  ( 0.000000000000000000, 0.000000000000000000, -1.000000000000000000 ) ) ;
#9879 = LINE ( 'NONE', #10279, #17093 ) ;
#9880 = EDGE_CURVE ( 'NONE', #18930, #19948, #8791, .T. ) ;
#9881 = ORIENTED_EDGE ( 'NONE', *, *, #17310, .F. ) ;
#9882 = COLOUR_RGB ( '', 0.31764706, 0.68627451, 0.89019608) ;
#9883 = ORIENTED_EDGE ( 'NONE', *, *, #9072, .T. ) ;
#9884 = ORIENTED_EDGE ( 'NONE', *, *, #19355, .T. ) ;
#9885 = EDGE_CURVE ( 'NONE', #4994, #758, #5493, .T. ) ;
#9886 = ORIENTED_EDGE ( 'NONE', *, *, #10914, .T. ) ;
#9887 = LINE ( 'NONE', #16199, #14356 ) ;
#9888 = CARTESIAN_POINT ( 'NONE',  ( -82.18192946989243808, 216.7545334744432921, 490.5655098179832976 ) ) ;
#9889 = LINE ( 'NONE', #2029, #17885 ) ;
#9890 = EDGE_CURVE ( 'NONE', #2920, #14515, #15016, .T. ) ;
#9891 = SURFACE_SIDE_STYLE ('',( #3517 ) ) ;
#9892 = AXIS2_PLACEMENT_3D ( 'NONE', #3185, #7921, #10918 ) ;
#9893 = DIRECTION ( 'NONE',  ( 0.000000000000000000, 0.000000000000000000, -1.000000000000000000 ) ) ;
#9894 = EDGE_CURVE ( 'NONE', #6680, #4513, #12406, .T. ) ;
#9895 = CIRCLE ( 'NONE', #3649, 14.27500000000000036 ) ;
#9896 = CARTESIAN_POINT ( 'NONE',  ( 22.99999999999998224, 10.00000000000000000, -31.99999999999998579 ) ) ;
#9897 = CARTESIAN_POINT ( 'NONE',  ( -34.99999999999996447, 11.00000000000000000, -40.00000000000000711 ) ) ;
#9898 =( GEOMETRIC_REPRESENTATION_CONTEXT ( 3 ) GLOBAL_UNCERTAINTY_ASSIGNED_CONTEXT ( ( #14926 ) ) GLOBAL_UNIT_ASSIGNED_CONTEXT ( ( #17213, #3097, #9389 ) ) REPRESENTATION_CONTEXT ( 'NONE', 'WORKASPACE' ) );
#9899 = CARTESIAN_POINT ( 'NONE',  ( 0.000000000000000000, -3.000000000000000000, 0.000000000000000000 ) ) ;
#9900 = EDGE_CURVE ( 'NONE', #19379, #19512, #14373, .T. ) ;
#9901 = FACE_BOUND ( 'NONE', #2117, .T. ) ;
#9902 =( NAMED_UNIT ( * ) PLANE_ANGLE_UNIT ( ) SI_UNIT ( $, .RADIAN. ) );
#9903 = VECTOR ( 'NONE', #11650, 1000.000000000000000 ) ;
#9904 = EDGE_CURVE ( 'NONE', #9830, #10847, #580, .T. ) ;
#9905 = SURFACE_STYLE_USAGE ( .BOTH. , #3724 ) ;
#9906 = CARTESIAN_POINT ( 'NONE',  ( 153.4893729001366864, 123.1299228374914634, 220.6387154965113382 ) ) ;
#9907 = VECTOR ( 'NONE', #3646, 1000.000000000000000 ) ;
#9908 = ORIENTED_EDGE ( 'NONE', *, *, #18671, .F. ) ;
#9909 = SURFACE_SIDE_STYLE ('',( #16326 ) ) ;
#9910 = UNCERTAINTY_MEASURE_WITH_UNIT (LENGTH_MEASURE( 1.000000000000000082E-05 ), #7028, 'distance_accuracy_value', 'NONE');
#9911 = ORIENTED_EDGE ( 'NONE', *, *, #12021, .T. ) ;
#9912 = PLANE ( 'NONE',  #8264 ) ;
#9913 = ORIENTED_EDGE ( 'NONE', *, *, #13024, .F. ) ;
#9914 = UNCERTAINTY_MEASURE_WITH_UNIT (LENGTH_MEASURE( 1.000000000000000082E-05 ), #10354, 'distance_accuracy_value', 'NONE');
#9915 = CYLINDRICAL_SURFACE ( 'NONE', #10674, 10.00000000000000888 ) ;
#9916 = DIRECTION ( 'NONE',  ( 1.000000000000000000, 0.000000000000000000, 0.000000000000000000 ) ) ;
#9917 = UNCERTAINTY_MEASURE_WITH_UNIT (LENGTH_MEASURE( 1.000000000000000082E-05 ), #7237, 'distance_accuracy_value', 'NONE');
#9918 = ORIENTED_EDGE ( 'NONE', *, *, #10094, .F. ) ;
#9919 = FILL_AREA_STYLE_COLOUR ( '', #14669 ) ;
#9920 = SURFACE_SIDE_STYLE ('',( #13039 ) ) ;
#9921 = LINE ( 'NONE', #6850, #9311 ) ;
#9922 = EDGE_CURVE ( 'NONE', #14767, #13515, #866, .T. ) ;
#9923 = SURFACE_STYLE_USAGE ( .BOTH. , #11367 ) ;
#9924 = CIRCLE ( 'NONE', #13218, 1.000000000000015987 ) ;
#9925 = DIRECTION ( 'NONE',  ( -1.000000000000000000, 0.000000000000000000, 0.000000000000000000 ) ) ;
#9926 = CYLINDRICAL_SURFACE ( 'NONE', #15986, 10.00000000000000888 ) ;
#9927 = EDGE_CURVE ( 'NONE', #4060, #2417, #4495, .T. ) ;
#9928 = ORIENTED_EDGE ( 'NONE', *, *, #1358, .T. ) ;
#9929 = DIRECTION ( 'NONE',  ( 0.000000000000000000, 1.000000000000000000, 0.000000000000000000 ) ) ;
#9930 = PLANE ( 'NONE',  #7595 ) ;
#9931 = SURFACE_STYLE_FILL_AREA ( #335 ) ;
#9932 = EDGE_CURVE ( 'NONE', #4918, #10186, #12430, .T. ) ;
#9933 = CARTESIAN_POINT ( 'NONE',  ( -22.99999999999999645, 68.00000000000000000, 31.00000000000003908 ) ) ;
#9934 = ORIENTED_EDGE ( 'NONE', *, *, #10295, .F. ) ;
#9935 = ORIENTED_EDGE ( 'NONE', *, *, #13421, .F. ) ;
#9936 = EDGE_LOOP ( 'NONE', ( #17753, #7487, #2061, #4826 ) ) ;
#9937 = VECTOR ( 'NONE', #5137, 1000.000000000000000 ) ;
#9938 = FILL_AREA_STYLE_COLOUR ( '', #9083 ) ;
#9939 = AXIS2_PLACEMENT_3D ( 'NONE', #14188, #15552, #14091 ) ;
#9940 = ORIENTED_EDGE ( 'NONE', *, *, #805, .T. ) ;
#9941 = UNCERTAINTY_MEASURE_WITH_UNIT (LENGTH_MEASURE( 1.000000000000000082E-05 ), #353, 'distance_accuracy_value', 'NONE');
#9942 = CARTESIAN_POINT ( 'NONE',  ( 78.48937290013662960, 1.675782865040797740E-14, -97.94896630388704750 ) ) ;
#9943 = CARTESIAN_POINT ( 'NONE',  ( 31.00000000000001776, 10.00000000000000000, -25.99999999999999645 ) ) ;
#9944 = ORIENTED_EDGE ( 'NONE', *, *, #10881, .F. ) ;
#9945 = DIRECTION ( 'NONE',  ( 1.000000000000000000, 0.000000000000000000, 0.000000000000000000 ) ) ;
#9946 = DIRECTION ( 'NONE',  ( 0.000000000000000000, 0.000000000000000000, -1.000000000000000000 ) ) ;
#9947 = DIRECTION ( 'NONE',  ( -1.000000000000000000, 0.000000000000000000, 0.000000000000000000 ) ) ;
#9948 = EDGE_CURVE ( 'NONE', #792, #9243, #10772, .T. ) ;
#9949 = CARTESIAN_POINT ( 'NONE',  ( -38.50085094405407204, 175.4489062796178871, 505.3921618609452935 ) ) ;
#9950 = ORIENTED_EDGE ( 'NONE', *, *, #19025, .T. ) ;
#9951 = FACE_OUTER_BOUND ( 'NONE', #2603, .T. ) ;
#9952 = CARTESIAN_POINT ( 'NONE',  ( 133.4893729001365443, 113.1299228374914634, 79.58252780074349175 ) ) ;
#9953 = FILL_AREA_STYLE_COLOUR ( '', #8635 ) ;
#9954 = AXIS2_PLACEMENT_3D ( 'NONE', #11523, #19437, #17802 ) ;
#9955 = ORIENTED_EDGE ( 'NONE', *, *, #16087, .F. ) ;
#9956 = CARTESIAN_POINT ( 'NONE',  ( 21.00000000000000000, 8.000000000000000000, 35.00000000000001421 ) ) ;
#9957 = AXIS2_PLACEMENT_3D ( 'NONE', #3377, #1822, #12455 ) ;
#9958 = DIRECTION ( 'NONE',  ( -0.000000000000000000, -1.000000000000000000, -0.000000000000000000 ) ) ;
#9959 = ORIENTED_EDGE ( 'NONE', *, *, #19666, .T. ) ;
#9960 = ORIENTED_EDGE ( 'NONE', *, *, #18795, .T. ) ;
#9961 = ORIENTED_EDGE ( 'NONE', *, *, #14193, .T. ) ;
#9962 = AXIS2_PLACEMENT_3D ( 'NONE', #3186, #15278, #3283 ) ;
#9963 = DIRECTION ( 'NONE',  ( 0.000000000000000000, 1.000000000000000000, 0.000000000000000000 ) ) ;
#9964 = EDGE_LOOP ( 'NONE', ( #20304, #3698, #959, #9061 ) ) ;
#9965 = DIRECTION ( 'NONE',  ( -3.854941057726249437E-16, 0.000000000000000000, -1.000000000000000000 ) ) ;
#9966 = SURFACE_SIDE_STYLE ('',( #3683 ) ) ;
#9967 = AXIS2_PLACEMENT_3D ( 'NONE', #14477, #6965, #8104 ) ;
#9968 = VERTEX_POINT ( 'NONE', #6038 ) ;
#9969 = DIRECTION ( 'NONE',  ( 0.000000000000000000, 1.000000000000000000, 0.000000000000000000 ) ) ;
#9970 = CARTESIAN_POINT ( 'NONE',  ( -23.00000000000003197, 0.000000000000000000, 37.00000000000000711 ) ) ;
#9971 = CARTESIAN_POINT ( 'NONE',  ( 0.09716098387576603546, 139.9221803985388419, 489.0003711267692665 ) ) ;
#9972 = PRODUCT_DEFINITION_FORMATION_WITH_SPECIFIED_SOURCE ( 'ANY', '', #4824, .NOT_KNOWN. ) ;
#9973 = CARTESIAN_POINT ( 'NONE',  ( -211.5106270998635409, 103.1299228374912360, 220.6387154965113382 ) ) ;
#9974 = STYLED_ITEM ( 'NONE', ( #5124 ), #3479 ) ;
#9975 = CARTESIAN_POINT ( 'NONE',  ( 0.000000000000000000, 80.91625508013694912, 250.0000000000000000 ) ) ;
#9976 = SHAPE_REPRESENTATION_RELATIONSHIP ( 'NONE' , 'NONE' ,  #17354, #9874 ) ;
#9977 = DIRECTION ( 'NONE',  ( -0.000000000000000000, -1.000000000000000000, -0.000000000000000000 ) ) ;
#9978 = CARTESIAN_POINT ( 'NONE',  ( -25.99999999999999645, 68.00000000000000000, -31.00000000000003197 ) ) ;
#9979 = CARTESIAN_POINT ( 'NONE',  ( 0.000000000000000000, 0.000000000000000000, 250.0000000000000000 ) ) ;
#9980 = ORIENTED_EDGE ( 'NONE', *, *, #18070, .F. ) ;
#9981 = DIRECTION ( 'NONE',  ( 0.000000000000000000, 0.000000000000000000, 1.000000000000000000 ) ) ;
#9982 = AXIS2_PLACEMENT_3D ( 'NONE', #19185, #10124, #8563 ) ;
#9983 = ORIENTED_EDGE ( 'NONE', *, *, #12055, .T. ) ;
#9984 = VERTEX_POINT ( 'NONE', #16772 ) ;
#9985 = EDGE_LOOP ( 'NONE', ( #16765, #4302, #4538, #8399 ) ) ;
#9986 = CLOSED_SHELL ( 'NONE', ( #12925, #736, #4868, #2897, #6193, #16557, #10768, #5523, #5969, #19198, #4856, #10258, #10481, #6937, #10527, #553, #7367, #13510, #19042, #15306 ) ) ;
#9987 = ORIENTED_EDGE ( 'NONE', *, *, #5276, .F. ) ;
#9988 = VECTOR ( 'NONE', #1398, 1000.000000000000000 ) ;
#9989 = ORIENTED_EDGE ( 'NONE', *, *, #2492, .T. ) ;
#9990 = EDGE_CURVE ( 'NONE', #16566, #17444, #2844, .T. ) ;
#9991 = FILL_AREA_STYLE_COLOUR ( '', #10741 ) ;
#9992 = LINE ( 'NONE', #19644, #19540 ) ;
#9993 = CARTESIAN_POINT ( 'NONE',  ( 458.8334540492693350, 167.8734308960555950, 250.0000000000000000 ) ) ;
#9994 = AXIS2_PLACEMENT_3D ( 'NONE', #4446, #15788, #11044 ) ;
#9995 = AXIS2_PLACEMENT_3D ( 'NONE', #6879, #18069, #19231 ) ;
#9996 = CARTESIAN_POINT ( 'NONE',  ( 30.99999999999997868, 10.00000000000000000, -30.99999999999999645 ) ) ;
#9997 = LINE ( 'NONE', #14945, #20270 ) ;
#9998 = LINE ( 'NONE', #2153, #19510 ) ;
#9999 = DIRECTION ( 'NONE',  ( 0.000000000000000000, 0.000000000000000000, -1.000000000000000000 ) ) ;
#10000 = CARTESIAN_POINT ( 'NONE',  ( 22.99999999999995737, 3.000000000000000000, -33.99999999999998579 ) ) ;
#10001 = DIRECTION ( 'NONE',  ( 0.000000000000000000, 1.000000000000000000, 0.000000000000000000 ) ) ;
#10002 = VECTOR ( 'NONE', #13364, 1000.000000000000000 ) ;
#10003 = EDGE_CURVE ( 'NONE', #9239, #14575, #13672, .T. ) ;
#10004 = STYLED_ITEM ( 'NONE', ( #6202 ), #343 ) ;
#10005 = FILL_AREA_STYLE_COLOUR ( '', #11679 ) ;
#10006 = CARTESIAN_POINT ( 'NONE',  ( -44.50085094405407915, 175.4489062796178871, 510.3921618609452935 ) ) ;
#10007 = VECTOR ( 'NONE', #19310, 1000.000000000000227 ) ;
#10008 = EDGE_CURVE ( 'NONE', #18431, #6703, #12317, .T. ) ;
#10009 = CIRCLE ( 'NONE', #14263, 4.999999999999997335 ) ;
#10010 = AXIS2_PLACEMENT_3D ( 'NONE', #12509, #14061, #6140 ) ;
#10011 = ADVANCED_FACE ( 'NONE', ( #2731 ), #15211, .F. ) ;
#10012 = ORIENTED_EDGE ( 'NONE', *, *, #11758, .F. ) ;
#10013 = CIRCLE ( 'NONE', #10335, 7.999999999999996447 ) ;
#10014 = LINE ( 'NONE', #5278, #12343 ) ;
#10015 = ORIENTED_EDGE ( 'NONE', *, *, #15614, .F. ) ;
#10016 = ADVANCED_FACE ( 'NONE', ( #1248 ), #20021, .T. ) ;
#10017 = CIRCLE ( 'NONE', #16616, 3.300000000000011369 ) ;
#10018 = ADVANCED_FACE ( 'NONE', ( #16973 ), #18606, .T. ) ;
#10019 = LINE ( 'NONE', #9816, #12660 ) ;
#10020 = CARTESIAN_POINT ( 'NONE',  ( 153.4893729001366864, 123.1299228374914634, 79.58252780074349175 ) ) ;
#10021 = ORIENTED_EDGE ( 'NONE', *, *, #13545, .T. ) ;
#10022 = VECTOR ( 'NONE', #18460, 1000.000000000000000 ) ;
#10023 = LINE ( 'NONE', #11977, #12708 ) ;
#10024 = CARTESIAN_POINT ( 'NONE',  ( -79.99999999999995737, 216.7545334744432921, 512.1946179577817020 ) ) ;
#10025 = CARTESIAN_POINT ( 'NONE',  ( -22.99999999999999645, 0.000000000000000000, 37.00000000000002132 ) ) ;
#10026 = AXIS2_PLACEMENT_3D ( 'NONE', #6460, #17874, #11185 ) ;
#10027 = AXIS2_PLACEMENT_3D ( 'NONE', #7162, #12179, #18454 ) ;
#10028 = VECTOR ( 'NONE', #18449, 1000.000000000000000 ) ;
#10029 = SURFACE_STYLE_USAGE ( .BOTH. , #17751 ) ;
#10030 = SURFACE_STYLE_FILL_AREA ( #3745 ) ;
#10031 = VECTOR ( 'NONE', #312, 1000.000000000000000 ) ;
#10032 =( LENGTH_UNIT ( ) NAMED_UNIT ( * ) SI_UNIT ( .MILLI., .METRE. ) );
#10033 = EDGE_CURVE ( 'NONE', #3885, #12344, #15454, .T. ) ;
#10034 = ORIENTED_EDGE ( 'NONE', *, *, #9228, .T. ) ;
#10035 = CARTESIAN_POINT ( 'NONE',  ( -3.000000000000000000, 6.000000000000000000, 3.000000000000000000 ) ) ;
#10036 = DIRECTION ( 'NONE',  ( 1.000000000000000000, 0.000000000000000000, 0.000000000000000000 ) ) ;
#10037 = DIRECTION ( 'NONE',  ( 0.000000000000000000, 0.000000000000000000, -1.000000000000000000 ) ) ;
#10038 = CONTEXT_DEPENDENT_SHAPE_REPRESENTATION ( #10246, #4483 ) ;
#10039 = STYLED_ITEM ( 'NONE', ( #13816 ), #1644 ) ;
#10040 = AXIS2_PLACEMENT_3D ( 'NONE', #8223, #11611, #14601 ) ;
#10041 = VERTEX_POINT ( 'NONE', #1158 ) ;
#10042 = ORIENTED_EDGE ( 'NONE', *, *, #10117, .F. ) ;
#10043 = EDGE_CURVE ( 'NONE', #19129, #2599, #2084, .T. ) ;
#10044 = AXIS2_PLACEMENT_3D ( 'NONE', #14248, #8186, #8081 ) ;
#10045 = VERTEX_POINT ( 'NONE', #5735 ) ;
#10046 = CIRCLE ( 'NONE', #5770, 1.000000000000000000 ) ;
#10047 = CARTESIAN_POINT ( 'NONE',  ( 39.99999999999999289, 0.000000000000000000, -26.00000000000000000 ) ) ;
#10048 = VECTOR ( 'NONE', #17457, 1000.000000000000000 ) ;
#10049 = ORIENTED_EDGE ( 'NONE', *, *, #7423, .F. ) ;
#10050 = SURFACE_SIDE_STYLE ('',( #3560 ) ) ;
#10051 = LINE ( 'NONE', #9943, #4279 ) ;
#10052 = ORIENTED_EDGE ( 'NONE', *, *, #11529, .T. ) ;
#10053 = DIRECTION ( 'NONE',  ( 0.000000000000000000, 1.000000000000000000, 0.000000000000000000 ) ) ;
#10054 = STYLED_ITEM ( 'NONE', ( #3423 ), #1836 ) ;
#10055 = VECTOR ( 'NONE', #1352, 1000.000000000000000 ) ;
#10056 = SURFACE_SIDE_STYLE ('',( #5316 ) ) ;
#10057 = DIRECTION ( 'NONE',  ( 0.000000000000000000, -0.7071067811865198172, -0.7071067811865753283 ) ) ;
#10058 = DIRECTION ( 'NONE',  ( 1.000000000000000000, 0.000000000000000000, 0.000000000000000000 ) ) ;
#10059 = ORIENTED_EDGE ( 'NONE', *, *, #5716, .F. ) ;
#10060 =( NAMED_UNIT ( * ) PLANE_ANGLE_UNIT ( ) SI_UNIT ( $, .RADIAN. ) );
#10061 = CARTESIAN_POINT ( 'NONE',  ( -40.00000000000000000, 68.00000000000000000, 26.00000000000000355 ) ) ;
#10062 =( NAMED_UNIT ( * ) SI_UNIT ( $, .STERADIAN. ) SOLID_ANGLE_UNIT ( ) );
#10063 = AXIS2_PLACEMENT_3D ( 'NONE', #11569, #5392, #8680 ) ;
#10064 = DIRECTION ( 'NONE',  ( 0.000000000000000000, 1.000000000000000000, 0.000000000000000000 ) ) ;
#10065 = EDGE_CURVE ( 'NONE', #975, #5571, #5930, .T. ) ;
#10066 = ORIENTED_EDGE ( 'NONE', *, *, #11697, .F. ) ;
#10067 = ORIENTED_EDGE ( 'NONE', *, *, #14666, .F. ) ;
#10068 = AXIS2_PLACEMENT_3D ( 'NONE', #11078, #15937, #1784 ) ;
#10069 = ORIENTED_EDGE ( 'NONE', *, *, #19571, .F. ) ;
#10070 = ORIENTED_EDGE ( 'NONE', *, *, #12184, .F. ) ;
#10071 = CYLINDRICAL_SURFACE ( 'NONE', #4008, 8.000000000000000000 ) ;
#10072 = DIRECTION ( 'NONE',  ( -0.000000000000000000, -1.000000000000000000, -0.000000000000000000 ) ) ;
#10073 = VERTEX_POINT ( 'NONE', #12211 ) ;
#10074 = DIRECTION ( 'NONE',  ( -0.000000000000000000, -1.000000000000000000, -0.000000000000000000 ) ) ;
#10075 = LINE ( 'NONE', #16083, #12926 ) ;
#10076 = VERTEX_POINT ( 'NONE', #18486 ) ;
#10077 = DIRECTION ( 'NONE',  ( 0.000000000000000000, 0.000000000000000000, -1.000000000000000000 ) ) ;
#10078 = CARTESIAN_POINT ( 'NONE',  ( 25.99999999999996092, 3.000000000000000000, 31.00000000000004263 ) ) ;
#10079 = VECTOR ( 'NONE', #19156, 1000.000000000000000 ) ;
#10080 = FILL_AREA_STYLE ('',( #11829 ) ) ;
#10081 = CARTESIAN_POINT ( 'NONE',  ( 0.000000000000000000, 66.00000000000000000, 0.9999999999999958922 ) ) ;
#10082 = CARTESIAN_POINT ( 'NONE',  ( -6.662140296159640225E-13, 139.7703989349544145, 490.5655098179848892 ) ) ;
#10083 = CONICAL_SURFACE ( 'NONE', #10068, 12.64907335584850046, 0.003530080289784348537 ) ;
#10084 = DIRECTION ( 'NONE',  ( -1.000000000000000000, 0.000000000000000000, -0.000000000000000000 ) ) ;
#10085 = LINE ( 'NONE', #5449, #6004 ) ;
#10086 = DIRECTION ( 'NONE',  ( -1.000000000000000000, -1.141265444721583757E-16, 0.000000000000000000 ) ) ;
#10087 = ORIENTED_EDGE ( 'NONE', *, *, #6681, .F. ) ;
#10088 = CARTESIAN_POINT ( 'NONE',  ( 25.99999999999999645, 11.00000000000000000, 40.00000000000000711 ) ) ;
#10089 = FACE_OUTER_BOUND ( 'NONE', #6956, .T. ) ;
#10090 = ORIENTED_EDGE ( 'NONE', *, *, #6071, .T. ) ;
#10091 = PRESENTATION_LAYER_ASSIGNMENT (  '', '', ( #19804 ) ) ;
#10092 = ORIENTED_EDGE ( 'NONE', *, *, #3452, .T. ) ;
#10093 = ORIENTED_EDGE ( 'NONE', *, *, #19556, .F. ) ;
#10094 = EDGE_CURVE ( 'NONE', #3589, #6194, #2831, .T. ) ;
#10095 = VERTEX_POINT ( 'NONE', #19214 ) ;
#10096 = ORIENTED_EDGE ( 'NONE', *, *, #6559, .F. ) ;
#10097 = CARTESIAN_POINT ( 'NONE',  ( -78.99999999999995737, 139.2066006846527841, 488.2525619656395861 ) ) ;
#10098 = AXIS2_PLACEMENT_3D ( 'NONE', #8153, #14424, #16602 ) ;
#10099 = DIRECTION ( 'NONE',  ( 0.000000000000000000, 0.000000000000000000, 1.000000000000000000 ) ) ;
#10100 = CARTESIAN_POINT ( 'NONE',  ( -33.00000000000000000, 10.00000000000000000, -22.00000000000000355 ) ) ;
#10101 = DIRECTION ( 'NONE',  ( 0.000000000000000000, 0.000000000000000000, -1.000000000000000000 ) ) ;
#10102 = LINE ( 'NONE', #5467, #11168 ) ;
#10103 = DIRECTION ( 'NONE',  ( 1.000000000000000000, 0.000000000000000000, 0.000000000000000000 ) ) ;
#10104 = CARTESIAN_POINT ( 'NONE',  ( -20.00000000000003197, 3.000000000000000000, 37.00000000000000711 ) ) ;
#10105 = CARTESIAN_POINT ( 'NONE',  ( 35.99999999999999289, 8.000000000000000000, 21.99999999999999645 ) ) ;
#10106 = CARTESIAN_POINT ( 'NONE',  ( -39.99999999999997868, 3.000000000000000000, 26.00000000000000355 ) ) ;
#10107 = DIRECTION ( 'NONE',  ( 1.000000000000000000, -0.000000000000000000, -0.000000000000000000 ) ) ;
#10108 = EDGE_CURVE ( 'NONE', #3089, #10871, #15835, .T. ) ;
#10109 = SURFACE_SIDE_STYLE ('',( #5376 ) ) ;
#10110 = VERTEX_POINT ( 'NONE', #45 ) ;
#10111 = EDGE_LOOP ( 'NONE', ( #14154, #14275, #11074, #6741, #14265 ) ) ;
#10112 = DIRECTION ( 'NONE',  ( 1.000000000000000000, 0.000000000000000000, 0.000000000000000000 ) ) ;
#10113 = UNCERTAINTY_MEASURE_WITH_UNIT (LENGTH_MEASURE( 1.000000000000000082E-05 ), #18578, 'distance_accuracy_value', 'NONE');
#10114 = ORIENTED_EDGE ( 'NONE', *, *, #3241, .T. ) ;
#10115 = ORIENTED_EDGE ( 'NONE', *, *, #7123, .T. ) ;
#10116 = VERTEX_POINT ( 'NONE', #3461 ) ;
#10117 = EDGE_CURVE ( 'NONE', #9449, #12228, #10338, .T. ) ;
#10118 = VECTOR ( 'NONE', #900, 1000.000000000000000 ) ;
#10119 = UNCERTAINTY_MEASURE_WITH_UNIT (LENGTH_MEASURE( 1.000000000000000082E-05 ), #19963, 'distance_accuracy_value', 'NONE');
#10120 = CARTESIAN_POINT ( 'NONE',  ( -64.99999999999995737, 317.7545334744432353, 475.1454018718993098 ) ) ;
#10121 = ORIENTED_EDGE ( 'NONE', *, *, #10982, .T. ) ;
#10122 = CARTESIAN_POINT ( 'NONE',  ( 2.181929469892980755, 147.7545334744432921, 496.6642397995873921 ) ) ;
#10123 = FILL_AREA_STYLE_COLOUR ( '', #16629 ) ;
#10124 = DIRECTION ( 'NONE',  ( -1.962615573354757393E-14, -0.7071067811865614505, 0.7071067811865336949 ) ) ;
#10125 = EDGE_CURVE ( 'NONE', #4967, #14468, #11176, .T. ) ;
#10126 = CARTESIAN_POINT ( 'NONE',  ( -19.00000000000001776, 8.000000000000000000, 40.00000000000000711 ) ) ;
#10127 = CARTESIAN_POINT ( 'NONE',  ( -1.387778780781445676E-14, 138.7545334744432637, 500.8237260975782874 ) ) ;
#10128 = CARTESIAN_POINT ( 'NONE',  ( 423.8334540492694487, 191.8198460455371333, 225.0057801310552463 ) ) ;
#10129 = DIRECTION ( 'NONE',  ( -3.854941057726247958E-16, 0.000000000000000000, 1.000000000000000000 ) ) ;
#10130 = EDGE_LOOP ( 'NONE', ( #17969, #16488, #4330, #12362 ) ) ;
#10131 = CARTESIAN_POINT ( 'NONE',  ( 0.000000000000000000, 313.8311070602663904, -142.2176018917206761 ) ) ;
#10132 = CARTESIAN_POINT ( 'NONE',  ( -34.99999999999998579, 0.000000000000000000, 21.00000000000000355 ) ) ;
#10133 = CARTESIAN_POINT ( 'NONE',  ( 26.00000000000000000, 19.00000000000000000, -40.00000000000000711 ) ) ;
#10134 = EDGE_CURVE ( 'NONE', #8671, #12704, #17895, .T. ) ;
#10135 = AXIS2_PLACEMENT_3D ( 'NONE', #14503, #377, #3596 ) ;
#10136 = EDGE_CURVE ( 'NONE', #10482, #5907, #3246, .T. ) ;
#10137 = ORIENTED_EDGE ( 'NONE', *, *, #13156, .F. ) ;
#10138 = ORIENTED_EDGE ( 'NONE', *, *, #12267, .T. ) ;
#10139 = ADVANCED_FACE ( 'NONE', ( #1882 ), #12625, .F. ) ;
#10140 = ORIENTED_EDGE ( 'NONE', *, *, #18304, .F. ) ;
#10141 = PRESENTATION_STYLE_ASSIGNMENT (( #5212 ) ) ;
#10142 = CARTESIAN_POINT ( 'NONE',  ( 31.81980515339464333, 8.000000000000000000, -31.81980515339463622 ) ) ;
#10143 = EDGE_LOOP ( 'NONE', ( #3529, #15004 ) ) ;
#10144 = DIRECTION ( 'NONE',  ( -0.000000000000000000, 0.000000000000000000, -1.000000000000000000 ) ) ;
#10145 =( NAMED_UNIT ( * ) PLANE_ANGLE_UNIT ( ) SI_UNIT ( $, .RADIAN. ) );
#10146 = DIRECTION ( 'NONE',  ( 1.000000000000000000, 5.889072920838430686E-16, -0.000000000000000000 ) ) ;
#10147 = EDGE_CURVE ( 'NONE', #738, #14419, #17262, .T. ) ;
#10148 = CARTESIAN_POINT ( 'NONE',  ( 53.48937290013659407, 211.0574367717017594, 346.4752554294135507 ) ) ;
#10149 = ORIENTED_EDGE ( 'NONE', *, *, #181, .T. ) ;
#10150 = CARTESIAN_POINT ( 'NONE',  ( 88.88953019741013861, 80.91625508013694912, 245.0000000000000000 ) ) ;
#10151 = PRESENTATION_STYLE_ASSIGNMENT (( #13160 ) ) ;
#10152 = DIRECTION ( 'NONE',  ( 0.000000000000000000, 1.000000000000000000, 0.000000000000000000 ) ) ;
#10153 = DIRECTION ( 'NONE',  ( -0.000000000000000000, -0.000000000000000000, 1.000000000000000000 ) ) ;
#10154 = EDGE_CURVE ( 'NONE', #10866, #4282, #4895, .T. ) ;
#10155 = DIRECTION ( 'NONE',  ( 1.000000000000000000, -0.000000000000000000, -0.000000000000000000 ) ) ;
#10156 = ORIENTED_EDGE ( 'NONE', *, *, #13297, .T. ) ;
#10157 = CONICAL_SURFACE ( 'NONE', #603, 12.97499999999999964, 0.5543074962015517304 ) ;
#10158 = EDGE_LOOP ( 'NONE', ( #14150, #12550 ) ) ;
#10159 = ORIENTED_EDGE ( 'NONE', *, *, #288, .F. ) ;
#10160 = ORIENTED_EDGE ( 'NONE', *, *, #7279, .F. ) ;
#10161 = FACE_BOUND ( 'NONE', #12297, .T. ) ;
#10162 = DIRECTION ( 'NONE',  ( -1.000000000000000000, -2.135044278125301096E-16, -0.000000000000000000 ) ) ;
#10163 = VERTEX_POINT ( 'NONE', #11081 ) ;
#10164 = DIRECTION ( 'NONE',  ( 0.000000000000000000, 0.000000000000000000, 1.000000000000000000 ) ) ;
#10165 = EDGE_CURVE ( 'NONE', #8072, #3481, #18550, .T. ) ;
#10166 = LINE ( 'NONE', #3795, #5281 ) ;
#10167 = DIRECTION ( 'NONE',  ( 1.000000000000000000, 0.000000000000000000, 0.000000000000000000 ) ) ;
#10168 = CARTESIAN_POINT ( 'NONE',  ( 0.1728887654703882282, 138.9434236829201836, 489.1421846862349412 ) ) ;
#10169 = STYLED_ITEM ( 'NONE', ( #5543 ), #5371 ) ;
#10170 = CARTESIAN_POINT ( 'NONE',  ( 0.000000000000000000, 306.0487089519832011, -80.00000000000380851 ) ) ;
#10171 = ADVANCED_FACE ( 'NONE', ( #3347 ), #9621, .F. ) ;
#10172 = CARTESIAN_POINT ( 'NONE',  ( -79.99999999999995737, 152.4824555358011082, 477.3411705753777596 ) ) ;
#10173 = DIRECTION ( 'NONE',  ( -1.000000000000000000, 0.000000000000000000, 0.000000000000000000 ) ) ;
#10174 = UNCERTAINTY_MEASURE_WITH_UNIT (LENGTH_MEASURE( 1.000000000000000082E-05 ), #15376, 'distance_accuracy_value', 'NONE');
#10175 = DIRECTION ( 'NONE',  ( 1.000000000000000000, 0.000000000000000000, 0.000000000000000000 ) ) ;
#10176 = DIRECTION ( 'NONE',  ( 1.000000000000000000, 5.889072920838430686E-16, -0.000000000000000000 ) ) ;
#10177 = VERTEX_POINT ( 'NONE', #250 ) ;
#10178 = EDGE_CURVE ( 'NONE', #4579, #17060, #6745, .T. ) ;
#10179 = CARTESIAN_POINT ( 'NONE',  ( -78.99999999999995737, 152.4824555358011082, 477.3411705753777596 ) ) ;
#10180 = EDGE_LOOP ( 'NONE', ( #16837, #18045, #9247, #2692, #10773 ) ) ;
#10181 = AXIS2_PLACEMENT_3D ( 'NONE', #8978, #1402, #12467 ) ;
#10182 = AXIS2_PLACEMENT_3D ( 'NONE', #17923, #18109, #16494 ) ;
#10183 = EDGE_LOOP ( 'NONE', ( #12372, #5956, #18840, #2529 ) ) ;
#10184 = CIRCLE ( 'NONE', #17416, 3.283624802691453848 ) ;
#10185 = PRESENTATION_LAYER_ASSIGNMENT (  '', '', ( #311 ) ) ;
#10186 = VERTEX_POINT ( 'NONE', #5004 ) ;
#10187 = VERTEX_POINT ( 'NONE', #17361 ) ;
#10188 = DIRECTION ( 'NONE',  ( 1.000000000000000000, 2.135044278125300850E-16, -0.000000000000000000 ) ) ;
#10189 = CARTESIAN_POINT ( 'NONE',  ( -58.16843972078500258, 317.7545334744432353, 481.2863735482146126 ) ) ;
#10190 = CARTESIAN_POINT ( 'NONE',  ( -39.99999999999999289, 8.000000000000000000, -34.99999999999997868 ) ) ;
#10191 = LINE ( 'NONE', #11754, #949 ) ;
#10192 = DIRECTION ( 'NONE',  ( -1.000000000000000000, -0.000000000000000000, -0.000000000000000000 ) ) ;
#10193 = CARTESIAN_POINT ( 'NONE',  ( 21.99999999999998224, 6.000000000000000000, -35.99999999999999289 ) ) ;
#10194 = PRESENTATION_LAYER_ASSIGNMENT (  '', '', ( #3631 ) ) ;
#10195 = CARTESIAN_POINT ( 'NONE',  ( -80.04214025239892294, 139.0005848764406551, 488.9285551588898215 ) ) ;
#10196 = CIRCLE ( 'NONE', #4278, 2.000000000000001776 ) ;
#10197 = SURFACE_STYLE_FILL_AREA ( #8858 ) ;
#10198 = ADVANCED_FACE ( 'NONE', ( #17558, #3152, #8581, #2394, #6773 ), #13150, .F. ) ;
#10199 = VECTOR ( 'NONE', #10344, 1000.000000000000000 ) ;
#10200 = DIRECTION ( 'NONE',  ( -1.000000000000000000, -2.135044278125301096E-16, -0.000000000000000000 ) ) ;
#10201 = CARTESIAN_POINT ( 'NONE',  ( -79.99999999999995737, 138.7545334744432637, 509.3921618609452935 ) ) ;
#10202 = ORIENTED_EDGE ( 'NONE', *, *, #15949, .T. ) ;
#10203 = ORIENTED_EDGE ( 'NONE', *, *, #11567, .T. ) ;
#10204 = DIRECTION ( 'NONE',  ( 1.000000000000000000, -0.000000000000000000, 0.000000000000000000 ) ) ;
#10205 = ORIENTED_EDGE ( 'NONE', *, *, #19068, .T. ) ;
#10206 = VERTEX_POINT ( 'NONE', #18056 ) ;
#10207 = AXIS2_PLACEMENT_3D ( 'NONE', #13375, #12015, #19614 ) ;
#10208 = FILL_AREA_STYLE_COLOUR ( '', #19849 ) ;
#10209 = CIRCLE ( 'NONE', #7225, 10.00000000000000888 ) ;
#10210 = CARTESIAN_POINT ( 'NONE',  ( 25.99999999999996092, 0.000000000000000000, 40.00000000000000711 ) ) ;
#10211 = CARTESIAN_POINT ( 'NONE',  ( 31.00000000000003553, 19.00000000000000000, 25.99999999999999645 ) ) ;
#10212 = ORIENTED_EDGE ( 'NONE', *, *, #11437, .T. ) ;
#10213 = EDGE_CURVE ( 'NONE', #10931, #15732, #11698, .T. ) ;
#10214 = DIRECTION ( 'NONE',  ( 1.595148023886719315E-16, -1.000000000000000000, 0.000000000000000000 ) ) ;
#10215 = SURFACE_STYLE_USAGE ( .BOTH. , #5891 ) ;
#10216 = CYLINDRICAL_SURFACE ( 'NONE', #17544, 18.50000000000000000 ) ;
#10217 = DIRECTION ( 'NONE',  ( 0.000000000000000000, 1.000000000000000000, 7.137148015447440312E-15 ) ) ;
#10218 = CARTESIAN_POINT ( 'NONE',  ( -211.5106270998635409, 123.1299228374912644, 79.58252780074349175 ) ) ;
#10219 = LINE ( 'NONE', #3940, #16818 ) ;
#10220 = SURFACE_STYLE_FILL_AREA ( #10436 ) ;
#10221 = VERTEX_POINT ( 'NONE', #7167 ) ;
#10222 = DIRECTION ( 'NONE',  ( 1.000000000000000000, -0.000000000000000000, 0.000000000000000000 ) ) ;
#10223 = DIRECTION ( 'NONE',  ( -1.000000000000000000, -0.000000000000000000, -0.000000000000000000 ) ) ;
#10224 = VECTOR ( 'NONE', #9828, 1000.000000000000000 ) ;
#10225 = MECHANICAL_DESIGN_GEOMETRIC_PRESENTATION_REPRESENTATION (  '', ( #5905 ), #13162 ) ;
#10226 = ADVANCED_FACE ( 'NONE', ( #5508 ), #10233, .T. ) ;
#10227 = CARTESIAN_POINT ( 'NONE',  ( 463.8334540492693350, 191.8198460455371333, 168.2339398819845826 ) ) ;
#10228 = EDGE_CURVE ( 'NONE', #1247, #39, #19494, .T. ) ;
#10229 = ORIENTED_EDGE ( 'NONE', *, *, #11254, .F. ) ;
#10230 = ORIENTED_EDGE ( 'NONE', *, *, #819, .F. ) ;
#10231 = ORIENTED_EDGE ( 'NONE', *, *, #6471, .F. ) ;
#10232 = EDGE_CURVE ( 'NONE', #10073, #9264, #14875, .T. ) ;
#10233 = CYLINDRICAL_SURFACE ( 'NONE', #1755, 4.999999999999997335 ) ;
#10234 = VECTOR ( 'NONE', #19440, 1000.000000000000000 ) ;
#10235 = CARTESIAN_POINT ( 'NONE',  ( -36.00000000000000711, 8.000000000000000000, -22.00000000000000355 ) ) ;
#10236 = EDGE_LOOP ( 'NONE', ( #10244, #4002, #19418, #11416 ) ) ;
#10237 = FACE_OUTER_BOUND ( 'NONE', #10111, .T. ) ;
#10238 = CARTESIAN_POINT ( 'NONE',  ( -20.00000000000003197, 3.000000000000000000, 37.00000000000000711 ) ) ;
#10239 = EDGE_CURVE ( 'NONE', #17989, #18007, #17766, .T. ) ;
#10240 = UNCERTAINTY_MEASURE_WITH_UNIT (LENGTH_MEASURE( 1.000000000000000082E-05 ), #8408, 'distance_accuracy_value', 'NONE');
#10241 = PLANE ( 'NONE',  #2130 ) ;
#10242 = CARTESIAN_POINT ( 'NONE',  ( -20.99999999999999645, 8.000000000000000000, 31.00000000000003197 ) ) ;
#10243 = DIRECTION ( 'NONE',  ( 0.000000000000000000, -1.632680918566406547E-16, 1.000000000000000000 ) ) ;
#10244 = ORIENTED_EDGE ( 'NONE', *, *, #2166, .F. ) ;
#10245 = CARTESIAN_POINT ( 'NONE',  ( -31.81980515339462912, 0.000000000000000000, -28.51980515339464972 ) ) ;
#10246 =( REPRESENTATION_RELATIONSHIP ('NONE','NONE', #13279, #1922 ) REPRESENTATION_RELATIONSHIP_WITH_TRANSFORMATION ( #3548 )SHAPE_REPRESENTATION_RELATIONSHIP( ) );
#10247 = LINE ( 'NONE', #5917, #1632 ) ;
#10248 = DIRECTION ( 'NONE',  ( 0.000000000000000000, 0.000000000000000000, 1.000000000000000000 ) ) ;
#10249 = EDGE_CURVE ( 'NONE', #13105, #8449, #20198, .T. ) ;
#10250 = EDGE_CURVE ( 'NONE', #53, #5039, #17254, .T. ) ;
#10251 = PRESENTATION_STYLE_ASSIGNMENT (( #18074 ) ) ;
#10252 = ORIENTED_EDGE ( 'NONE', *, *, #3881, .T. ) ;
#10253 = STYLED_ITEM ( 'NONE', ( #8118 ), #17573 ) ;
#10254 = ORIENTED_EDGE ( 'NONE', *, *, #13166, .T. ) ;
#10255 = EDGE_CURVE ( 'NONE', #13429, #19208, #8378, .T. ) ;
#10256 = AXIS2_PLACEMENT_3D ( 'NONE', #9452, #19011, #7602 ) ;
#10257 = EDGE_LOOP ( 'NONE', ( #19642, #13846, #3789, #19582 ) ) ;
#10258 = ADVANCED_FACE ( 'NONE', ( #8301 ), #2089, .T. ) ;
#10259 = VERTEX_POINT ( 'NONE', #15393 ) ;
#10260 = EDGE_LOOP ( 'NONE', ( #2595, #6431 ) ) ;
#10261 = FACE_OUTER_BOUND ( 'NONE', #8207, .T. ) ;
#10262 = CARTESIAN_POINT ( 'NONE',  ( 0.000000000000000000, 65.20000000000000284, 0.9999999999999976685 ) ) ;
#10263 = VERTEX_POINT ( 'NONE', #9191 ) ;
#10264 = EDGE_CURVE ( 'NONE', #9564, #7792, #1223, .T. ) ;
#10265 = FILL_AREA_STYLE_COLOUR ( '', #5035 ) ;
#10266 = EDGE_CURVE ( 'NONE', #8092, #1837, #15293, .T. ) ;
#10267 = DIRECTION ( 'NONE',  ( -0.000000000000000000, -1.000000000000000000, -0.000000000000000000 ) ) ;
#10268 = LINE ( 'NONE', #10078, #13247 ) ;
#10269 = CARTESIAN_POINT ( 'NONE',  ( -1.301042606982605321E-14, 140.0734055309426083, 488.6914064109051878 ) ) ;
#10270 = CARTESIAN_POINT ( 'NONE',  ( -26.00000000000000355, 11.00000000000000000, 31.00000000000003553 ) ) ;
#10271 = DIRECTION ( 'NONE',  ( 0.000000000000000000, 0.000000000000000000, -1.000000000000000000 ) ) ;
#10272 = CARTESIAN_POINT ( 'NONE',  ( -37.00000000000000000, 68.00000000000000000, 23.00000000000000355 ) ) ;
#10273 = DIRECTION ( 'NONE',  ( 0.000000000000000000, 0.000000000000000000, 1.000000000000000000 ) ) ;
#10274 = FILL_AREA_STYLE_COLOUR ( '', #11264 ) ;
#10275 = AXIS2_PLACEMENT_3D ( 'NONE', #7371, #5920, #15196 ) ;
#10276 = DIRECTION ( 'NONE',  ( -0.000000000000000000, -1.000000000000000000, -0.000000000000000000 ) ) ;
#10277 = EDGE_CURVE ( 'NONE', #504, #2482, #9026, .T. ) ;
#10278 = LINE ( 'NONE', #16783, #20108 ) ;
#10279 = CARTESIAN_POINT ( 'NONE',  ( 0.000000000000000000, 313.8311070602663904, -142.2176018917206761 ) ) ;
#10280 = VERTEX_POINT ( 'NONE', #7468 ) ;
#10281 = DIRECTION ( 'NONE',  ( 0.000000000000000000, 0.000000000000000000, -1.000000000000000000 ) ) ;
#10282 = EDGE_LOOP ( 'NONE', ( #5673, #321 ) ) ;
#10283 = AXIS2_PLACEMENT_3D ( 'NONE', #12439, #17275, #6360 ) ;
#10284 = PRODUCT_DEFINITION_CONTEXT ( 'detailed design', #18282, 'design' ) ;
#10285 = ORIENTED_EDGE ( 'NONE', *, *, #10810, .T. ) ;
#10286 =( GEOMETRIC_REPRESENTATION_CONTEXT ( 3 ) GLOBAL_UNCERTAINTY_ASSIGNED_CONTEXT ( ( #292 ) ) GLOBAL_UNIT_ASSIGNED_CONTEXT ( ( #17456, #1572, #11180 ) ) REPRESENTATION_CONTEXT ( 'NONE', 'WORKASPACE' ) );
#10287 = VERTEX_POINT ( 'NONE', #16838 ) ;
#10288 = EDGE_CURVE ( 'NONE', #2504, #10095, #20107, .T. ) ;
#10289 = DIRECTION ( 'NONE',  ( -1.000000000000000000, -0.000000000000000000, -0.000000000000000000 ) ) ;
#10290 = LINE ( 'NONE', #11851, #15 ) ;
#10291 = DIRECTION ( 'NONE',  ( 1.000000000000000000, -4.371814833150063998E-14, -1.016981637791458695E-13 ) ) ;
#10292 = EDGE_CURVE ( 'NONE', #13536, #5483, #6009, .T. ) ;
#10293 = CIRCLE ( 'NONE', #12602, 10.00000000000000888 ) ;
#10294 = DIRECTION ( 'NONE',  ( -1.597771622610217359E-16, 1.000000000000000000, 0.000000000000000000 ) ) ;
#10295 = EDGE_CURVE ( 'NONE', #3014, #17794, #8993, .T. ) ;
#10296 = FILL_AREA_STYLE_COLOUR ( '', #18517 ) ;
#10297 = CARTESIAN_POINT ( 'NONE',  ( -37.00000000000000000, 68.00000000000000000, 23.00000000000000355 ) ) ;
#10298 = DIRECTION ( 'NONE',  ( 7.900838015626929923E-17, 8.586860021784410058E-33, -1.000000000000000000 ) ) ;
#10299 = AXIS2_PLACEMENT_3D ( 'NONE', #15545, #12647, #4911 ) ;
#10300 = CIRCLE ( 'NONE', #16571, 4.000000000000003553 ) ;
#10301 = CARTESIAN_POINT ( 'NONE',  ( 45.00000000000001421, 0.000000000000000000, 0.000000000000000000 ) ) ;
#10302 = CARTESIAN_POINT ( 'NONE',  ( 423.8334540492694487, 191.8198460455371333, 225.0057801310552463 ) ) ;
#10303 = CARTESIAN_POINT ( 'NONE',  ( 0.000000000000000000, 0.000000000000000000, 0.000000000000000000 ) ) ;
#10304 = CARTESIAN_POINT ( 'NONE',  ( 31.00000000000003553, 11.00000000000000000, 25.99999999999999645 ) ) ;
#10305 = CARTESIAN_POINT ( 'NONE',  ( 40.00000000000001421, -5.000000000000000888, -150.0000000000000000 ) ) ;
#10306 = CARTESIAN_POINT ( 'NONE',  ( -26.00000000000002132, 10.00000000000000000, 40.00000000000000711 ) ) ;
#10307 =( GEOMETRIC_REPRESENTATION_CONTEXT ( 3 ) GLOBAL_UNCERTAINTY_ASSIGNED_CONTEXT ( ( #12000 ) ) GLOBAL_UNIT_ASSIGNED_CONTEXT ( ( #8048, #209, #1623 ) ) REPRESENTATION_CONTEXT ( 'NONE', 'WORKASPACE' ) );
#10308 = VECTOR ( 'NONE', #8138, 1000.000000000000000 ) ;
#10309 = ORIENTED_EDGE ( 'NONE', *, *, #5580, .T. ) ;
#10310 = EDGE_LOOP ( 'NONE', ( #13386, #14137, #18209, #19746 ) ) ;
#10311 = DIRECTION ( 'NONE',  ( -0.000000000000000000, -1.000000000000000000, -0.000000000000000000 ) ) ;
#10312 = ORIENTED_EDGE ( 'NONE', *, *, #2217, .T. ) ;
#10313 = ORIENTED_EDGE ( 'NONE', *, *, #15811, .F. ) ;
#10314 =( GEOMETRIC_REPRESENTATION_CONTEXT ( 3 ) GLOBAL_UNCERTAINTY_ASSIGNED_CONTEXT ( ( #8673 ) ) GLOBAL_UNIT_ASSIGNED_CONTEXT ( ( #2988, #2885, #17109 ) ) REPRESENTATION_CONTEXT ( 'NONE', 'WORKASPACE' ) );
#10315 = AXIS2_PLACEMENT_3D ( 'NONE', #12964, #17576, #4604 ) ;
#10316 = ORIENTED_EDGE ( 'NONE', *, *, #17075, .F. ) ;
#10317 = LINE ( 'NONE', #16630, #20177 ) ;
#10318 = ADVANCED_FACE ( 'NONE', ( #13939 ), #12097, .T. ) ;
#10319 = LINE ( 'NONE', #7041, #668 ) ;
#10320 = CARTESIAN_POINT ( 'NONE',  ( 498.8334540492693918, 191.8198460455371333, 178.2339398819846110 ) ) ;
#10321 = DIRECTION ( 'NONE',  ( 1.000000000000000000, 0.000000000000000000, 3.328238341717372086E-14 ) ) ;
#10322 = CARTESIAN_POINT ( 'NONE',  ( -1.000000000000021094, 147.7545334744432921, 496.6642397995874489 ) ) ;
#10323 = CARTESIAN_POINT ( 'NONE',  ( -26.00000000000002842, 0.000000000000000000, 34.00000000000000711 ) ) ;
#10324 =( GEOMETRIC_REPRESENTATION_CONTEXT ( 3 ) GLOBAL_UNCERTAINTY_ASSIGNED_CONTEXT ( ( #19602 ) ) GLOBAL_UNIT_ASSIGNED_CONTEXT ( ( #5486, #7040, #8296 ) ) REPRESENTATION_CONTEXT ( 'NONE', 'WORKASPACE' ) );
#10325 = CARTESIAN_POINT ( 'NONE',  ( 0.6999999999999999556, 18.50000000000000000, 0.000000000000000000 ) ) ;
#10326 = CARTESIAN_POINT ( 'NONE',  ( -81.00000000000127898, 139.7703989349544997, 489.5655098179835818 ) ) ;
#10327 = DIRECTION ( 'NONE',  ( -1.000000000000000000, 0.000000000000000000, -0.000000000000000000 ) ) ;
#10328 = VERTEX_POINT ( 'NONE', #12288 ) ;
#10329 =( LENGTH_UNIT ( ) NAMED_UNIT ( * ) SI_UNIT ( .MILLI., .METRE. ) );
#10330 = CARTESIAN_POINT ( 'NONE',  ( 1.000000000001310063, 216.7545334744432921, 489.5655098179835818 ) ) ;
#10331 = CIRCLE ( 'NONE', #13637, 12.65000000000000036 ) ;
#10332 = VECTOR ( 'NONE', #20100, 1000.000000000000000 ) ;
#10333 = CARTESIAN_POINT ( 'NONE',  ( 10.00000000000000000, 301.0487089519837127, -150.0000000000038369 ) ) ;
#10334 = VECTOR ( 'NONE', #15043, 1000.000000000000000 ) ;
#10335 = AXIS2_PLACEMENT_3D ( 'NONE', #19786, #9182, #4455 ) ;
#10336 = AXIS2_PLACEMENT_3D ( 'NONE', #12139, #5771, #891 ) ;
#10337 = VERTEX_POINT ( 'NONE', #5908 ) ;
#10338 = CIRCLE ( 'NONE', #8033, 3.300000000000025135 ) ;
#10339 = EDGE_CURVE ( 'NONE', #2573, #3307, #12185, .T. ) ;
#10340 = VERTEX_POINT ( 'NONE', #10746 ) ;
#10341 = PRESENTATION_LAYER_ASSIGNMENT (  '', '', ( #8383 ) ) ;
#10342 = PLANE ( 'NONE',  #12018 ) ;
#10343 = VECTOR ( 'NONE', #13511, 1000.000000000000000 ) ;
#10344 = DIRECTION ( 'NONE',  ( 1.000000000000000000, 0.000000000000000000, 0.000000000000000000 ) ) ;
#10345 = UNCERTAINTY_MEASURE_WITH_UNIT (LENGTH_MEASURE( 1.000000000000000082E-05 ), #2788, 'distance_accuracy_value', 'NONE');
#10346 = ORIENTED_EDGE ( 'NONE', *, *, #2082, .T. ) ;
#10347 = DIRECTION ( 'NONE',  ( 1.000000000000000000, 9.815121534730717399E-17, 0.000000000000000000 ) ) ;
#10348 = CARTESIAN_POINT ( 'NONE',  ( -80.84381259993401159, 139.4861549369088038, 500.2186618848270996 ) ) ;
#10349 = FILL_AREA_STYLE_COLOUR ( '', #18510 ) ;
#10350 = LINE ( 'NONE', #16662, #488 ) ;
#10351 = CARTESIAN_POINT ( 'NONE',  ( -80.99999999999995737, 139.4861549369088323, 500.2186618848270996 ) ) ;
#10352 = CARTESIAN_POINT ( 'NONE',  ( -81.18192946989275072, 139.4861549369088323, 500.2186618848270996 ) ) ;
#10353 = MECHANICAL_DESIGN_GEOMETRIC_PRESENTATION_REPRESENTATION (  '', ( #15975 ), #19538 ) ;
#10354 =( LENGTH_UNIT ( ) NAMED_UNIT ( * ) SI_UNIT ( .MILLI., .METRE. ) );
#10355 = EDGE_LOOP ( 'NONE', ( #11098, #10229, #17101, #5720 ) ) ;
#10356 = DIRECTION ( 'NONE',  ( 1.000000000000000000, -0.000000000000000000, 0.000000000000000000 ) ) ;
#10357 = DIRECTION ( 'NONE',  ( -1.597771622610217359E-16, 1.000000000000000000, -0.000000000000000000 ) ) ;
#10358 = VECTOR ( 'NONE', #17527, 1000.000000000000000 ) ;
#10359 = ADVANCED_FACE ( 'NONE', ( #2601 ), #10342, .T. ) ;
#10360 = VECTOR ( 'NONE', #17046, 1000.000000000000000 ) ;
#10361 = ORIENTED_EDGE ( 'NONE', *, *, #8155, .F. ) ;
#10362 = CIRCLE ( 'NONE', #18252, 5.000000000000000888 ) ;
#10363 = VERTEX_POINT ( 'NONE', #16655 ) ;
#10364 = AXIS2_PLACEMENT_3D ( 'NONE', #8106, #12635, #11183 ) ;
#10365 = VERTEX_POINT ( 'NONE', #8802 ) ;
#10366 = AXIS2_PLACEMENT_3D ( 'NONE', #1109, #14962, #4331 ) ;
#10367 = DIRECTION ( 'NONE',  ( 0.000000000000000000, 1.000000000000000000, 0.000000000000000000 ) ) ;
#10368 = VECTOR ( 'NONE', #15840, 1000.000000000000000 ) ;
#10369 = ORIENTED_EDGE ( 'NONE', *, *, #18391, .T. ) ;
#10370 = CARTESIAN_POINT ( 'NONE',  ( -36.99999999999997868, 0.000000000000000000, -22.99999999999999645 ) ) ;
#10371 = CARTESIAN_POINT ( 'NONE',  ( 31.81980515339464333, 8.000000000000000000, 35.11980515339463693 ) ) ;
#10372 = AXIS2_PLACEMENT_3D ( 'NONE', #9065, #18639, #2861 ) ;
#10373 = ORIENTED_EDGE ( 'NONE', *, *, #11411, .F. ) ;
#10374 = SURFACE_STYLE_USAGE ( .BOTH. , #18386 ) ;
#10375 = EDGE_CURVE ( 'NONE', #19767, #6154, #934, .T. ) ;
#10376 = FILL_AREA_STYLE ('',( #10265 ) ) ;
#10377 = CARTESIAN_POINT ( 'NONE',  ( -36.00000000000000711, 10.00000000000000000, -22.00000000000000355 ) ) ;
#10378 = VECTOR ( 'NONE', #15544, 1000.000000000000000 ) ;
#10379 = DIRECTION ( 'NONE',  ( 0.000000000000000000, 0.000000000000000000, -1.000000000000000000 ) ) ;
#10380 = SHAPE_REPRESENTATION ( 'Servo-Bas', ( #2741 ), #14258 ) ;
#10381 = CARTESIAN_POINT ( 'NONE',  ( 111.4893729001366012, 127.7247684487574588, 357.7985149490353933 ) ) ;
#10382 = AXIS2_PLACEMENT_3D ( 'NONE', #15723, #16035, #9596 ) ;
#10383 = CARTESIAN_POINT ( 'NONE',  ( 35.99999999999999289, 6.000000000000000000, 17.99999999999998934 ) ) ;
#10384 = ADVANCED_FACE ( 'NONE', ( #5702 ), #16750, .T. ) ;
#10385 = DIRECTION ( 'NONE',  ( 0.000000000000000000, 1.000000000000000000, -0.000000000000000000 ) ) ;
#10386 = DIRECTION ( 'NONE',  ( 0.000000000000000000, -1.000000000000000000, 0.000000000000000000 ) ) ;
#10387 = CARTESIAN_POINT ( 'NONE',  ( -37.00000000000000711, 0.000000000000000000, -23.00000000000000000 ) ) ;
#10388 = DIRECTION ( 'NONE',  ( 0.000000000000000000, 0.000000000000000000, -1.000000000000000000 ) ) ;
#10389 = CARTESIAN_POINT ( 'NONE',  ( 143.0892156028631348, 80.91625508013694912, 245.0000000000000000 ) ) ;
#10390 = AXIS2_PLACEMENT_3D ( 'NONE', #1643, #3223, #4780 ) ;
#10391 = CYLINDRICAL_SURFACE ( 'NONE', #10843, 4.999999999999997335 ) ;
#10392 = CARTESIAN_POINT ( 'NONE',  ( 6.299999999999999822, -18.50000000000000000, -2.265596578422603396E-15 ) ) ;
#10393 = CARTESIAN_POINT ( 'NONE',  ( 423.8334540492694487, 191.8198460455371333, 215.0057801310552179 ) ) ;
#10394 = EDGE_LOOP ( 'NONE', ( #4685, #18624, #17201, #3733 ) ) ;
#10395 = PRESENTATION_LAYER_ASSIGNMENT (  '', '', ( #11706 ) ) ;
#10396 = EDGE_CURVE ( 'NONE', #2161, #18128, #18567, .T. ) ;
#10397 = DIRECTION ( 'NONE',  ( 1.000000000000000000, 0.000000000000000000, 0.000000000000000000 ) ) ;
#10398 = EDGE_CURVE ( 'NONE', #16269, #7792, #5816, .T. ) ;
#10399 = EDGE_LOOP ( 'NONE', ( #13660, #8475, #7376, #6196 ) ) ;
#10400 = ORIENTED_EDGE ( 'NONE', *, *, #18011, .F. ) ;
#10401 = VECTOR ( 'NONE', #17842, 1000.000000000000000 ) ;
#10402 = DIRECTION ( 'NONE',  ( -0.000000000000000000, 0.000000000000000000, 1.000000000000000000 ) ) ;
#10403 = DIRECTION ( 'NONE',  ( 0.000000000000000000, 0.000000000000000000, 1.000000000000000000 ) ) ;
#10404 = ADVANCED_FACE ( 'NONE', ( #1753 ), #17337, .T. ) ;
#10405 = LINE ( 'NONE', #13499, #4732 ) ;
#10406 = DIRECTION ( 'NONE',  ( 0.000000000000000000, -1.000000000000000000, 0.000000000000000000 ) ) ;
#10407 = CIRCLE ( 'NONE', #18936, 10.00000000000000888 ) ;
#10408 = CARTESIAN_POINT ( 'NONE',  ( 458.8334540492693350, 191.8198460455371333, 14.99421986894475012 ) ) ;
#10409 = DIRECTION ( 'NONE',  ( -1.000000000000000000, -3.816214432251725906E-17, 4.784675105189226675E-17 ) ) ;
#10410 = DIRECTION ( 'NONE',  ( -0.7327934916262990317, 0.6804510993672779895, 0.000000000000000000 ) ) ;
#10411 = CARTESIAN_POINT ( 'NONE',  ( 25.99999999999999645, 68.00000000000000000, 40.00000000000002132 ) ) ;
#10412 = EDGE_CURVE ( 'NONE', #2362, #12373, #8176, .T. ) ;
#10413 = LINE ( 'NONE', #4233, #4973 ) ;
#10414 = CARTESIAN_POINT ( 'NONE',  ( 21.00000000000000000, 19.00000000000000000, -31.00000000000003908 ) ) ;
#10415 = CARTESIAN_POINT ( 'NONE',  ( 53.48937290013660828, 127.7247684487574020, 357.7985149490353933 ) ) ;
#10416 = DIRECTION ( 'NONE',  ( -1.000000000000000000, 0.000000000000000000, -0.000000000000000000 ) ) ;
#10417 = EDGE_CURVE ( 'NONE', #10187, #12712, #14240, .T. ) ;
#10418 = CIRCLE ( 'NONE', #4830, 10.00000000000000888 ) ;
#10419 = EDGE_LOOP ( 'NONE', ( #10954, #8268, #4547, #533 ) ) ;
#10420 = CIRCLE ( 'NONE', #8457, 10.00000000000000888 ) ;
#10421 = ORIENTED_EDGE ( 'NONE', *, *, #18391, .F. ) ;
#10422 = ORIENTED_EDGE ( 'NONE', *, *, #13762, .F. ) ;
#10423 = FILL_AREA_STYLE_COLOUR ( '', #1127 ) ;
#10424 = VERTEX_POINT ( 'NONE', #12404 ) ;
#10425 = ORIENTED_EDGE ( 'NONE', *, *, #7873, .T. ) ;
#10426 = DIRECTION ( 'NONE',  ( 1.000000000000000000, 0.000000000000000000, 0.000000000000000000 ) ) ;
#10427 = FACE_OUTER_BOUND ( 'NONE', #14894, .T. ) ;
#10428 = CARTESIAN_POINT ( 'NONE',  ( 26.00000000000000711, 0.000000000000000000, -31.00000000000002487 ) ) ;
#10429 = LINE ( 'NONE', #13723, #14447 ) ;
#10430 = DIRECTION ( 'NONE',  ( 1.000000000000000000, 5.889072920838430686E-16, -0.000000000000000000 ) ) ;
#10431 = LINE ( 'NONE', #11778, #19499 ) ;
#10432 = ADVANCED_FACE ( 'NONE', ( #7854 ), #14351, .T. ) ;
#10433 = SURFACE_STYLE_USAGE ( .BOTH. , #1010 ) ;
#10434 = CARTESIAN_POINT ( 'NONE',  ( 31.00000000000003908, 19.00000000000000000, -26.00000000000000355 ) ) ;
#10435 = CARTESIAN_POINT ( 'NONE',  ( -80.51861556725816627, 138.8636137914787696, 489.4457938216992261 ) ) ;
#10436 = FILL_AREA_STYLE ('',( #15170 ) ) ;
#10437 = VERTEX_POINT ( 'NONE', #4661 ) ;
#10438 = CARTESIAN_POINT ( 'NONE',  ( -31.00000000000006395, 19.00000000000000000, 20.99999999999998934 ) ) ;
#10439 = LINE ( 'NONE', #7461, #2095 ) ;
#10440 = EDGE_CURVE ( 'NONE', #19612, #19303, #2771, .T. ) ;
#10441 = PRESENTATION_STYLE_ASSIGNMENT (( #13827 ) ) ;
#10442 = ORIENTED_EDGE ( 'NONE', *, *, #3852, .T. ) ;
#10443 = ORIENTED_EDGE ( 'NONE', *, *, #4440, .F. ) ;
#10444 = DIRECTION ( 'NONE',  ( -0.000000000000000000, -1.000000000000000000, -0.000000000000000000 ) ) ;
#10445 = DIRECTION ( 'NONE',  ( 0.000000000000000000, 0.000000000000000000, -1.000000000000000000 ) ) ;
#10446 = ORIENTED_EDGE ( 'NONE', *, *, #2027, .F. ) ;
#10447 = DIRECTION ( 'NONE',  ( 1.000000000000000000, 0.000000000000000000, -0.000000000000000000 ) ) ;
#10448 =( LENGTH_UNIT ( ) NAMED_UNIT ( * ) SI_UNIT ( .MILLI., .METRE. ) );
#10449 = CARTESIAN_POINT ( 'NONE',  ( 498.8334540492693918, 167.8734308960555950, 250.0000000000000000 ) ) ;
#10450 = CARTESIAN_POINT ( 'NONE',  ( 53.48937290013659407, 129.7247684487574588, 283.6050404526570219 ) ) ;
#10451 =( NAMED_UNIT ( * ) SI_UNIT ( $, .STERADIAN. ) SOLID_ANGLE_UNIT ( ) );
#10452 = STYLED_ITEM ( 'NONE', ( #6080 ), #3975 ) ;
#10453 = VERTEX_POINT ( 'NONE', #10846 ) ;
#10454 =( LENGTH_UNIT ( ) NAMED_UNIT ( * ) SI_UNIT ( .MILLI., .METRE. ) );
#10455 = DIRECTION ( 'NONE',  ( -1.000000000000000000, 0.000000000000000000, 0.000000000000000000 ) ) ;
#10456 = DIRECTION ( 'NONE',  ( 0.000000000000000000, 0.000000000000000000, 1.000000000000000000 ) ) ;
#10457 = APPLICATION_PROTOCOL_DEFINITION ( 'draft international standard', 'automotive_design', 1998, #4217 ) ;
#10458 = ADVANCED_FACE ( 'NONE', ( #18865 ), #14135, .T. ) ;
#10459 = VERTEX_POINT ( 'NONE', #9497 ) ;
#10460 = ORIENTED_EDGE ( 'NONE', *, *, #1066, .T. ) ;
#10461 = LINE ( 'NONE', #7375, #10606 ) ;
#10462 = ORIENTED_EDGE ( 'NONE', *, *, #11174, .T. ) ;
#10463 = ORIENTED_EDGE ( 'NONE', *, *, #2833, .T. ) ;
#10464 = ORIENTED_EDGE ( 'NONE', *, *, #17713, .F. ) ;
#10465 = CARTESIAN_POINT ( 'NONE',  ( 0.000000000000000000, 167.9162550801369491, 0.000000000000000000 ) ) ;
#10466 = CIRCLE ( 'NONE', #2211, 3.300000000000011369 ) ;
#10467 = VERTEX_POINT ( 'NONE', #7955 ) ;
#10468 = DIRECTION ( 'NONE',  ( 1.000000000000000000, 0.000000000000000000, -0.000000000000000000 ) ) ;
#10469 = DIRECTION ( 'NONE',  ( 0.000000000000000000, 0.000000000000000000, -1.000000000000000000 ) ) ;
#10470 = DIRECTION ( 'NONE',  ( -0.000000000000000000, -1.000000000000000000, -0.000000000000000000 ) ) ;
#10471 =( LENGTH_UNIT ( ) NAMED_UNIT ( * ) SI_UNIT ( .MILLI., .METRE. ) );
#10472 = EDGE_CURVE ( 'NONE', #12727, #4894, #12811, .T. ) ;
#10473 = CARTESIAN_POINT ( 'NONE',  ( -39.99999999999997868, 3.000000000000000000, -19.99999999999999645 ) ) ;
#10474 = CARTESIAN_POINT ( 'NONE',  ( 36.99999999999999289, 0.000000000000000000, 22.99999999999999645 ) ) ;
#10475 = CARTESIAN_POINT ( 'NONE',  ( 1.181929469854658965, 139.7545334744432637, -9.119545354731954390E-14 ) ) ;
#10476 = CARTESIAN_POINT ( 'NONE',  ( 21.00000000000000000, 19.00000000000000000, 35.00000000000001421 ) ) ;
#10477 = CARTESIAN_POINT ( 'NONE',  ( 10.00000000000000000, 376.0487089519831443, -75.00000000000331113 ) ) ;
#10478 = DIRECTION ( 'NONE',  ( 0.000000000000000000, -0.000000000000000000, 1.000000000000000000 ) ) ;
#10479 =( NAMED_UNIT ( * ) PLANE_ANGLE_UNIT ( ) SI_UNIT ( $, .RADIAN. ) );
#10480 = FILL_AREA_STYLE ('',( #10583 ) ) ;
#10481 = ADVANCED_FACE ( 'NONE', ( #10952 ), #17427, .F. ) ;
#10482 = VERTEX_POINT ( 'NONE', #3535 ) ;
#10483 = UNCERTAINTY_MEASURE_WITH_UNIT (LENGTH_MEASURE( 1.000000000000000082E-05 ), #15679, 'distance_accuracy_value', 'NONE');
#10484 = ORIENTED_EDGE ( 'NONE', *, *, #19210, .F. ) ;
#10485 = EDGE_CURVE ( 'NONE', #18945, #1341, #17837, .T. ) ;
#10486 = ORIENTED_EDGE ( 'NONE', *, *, #7392, .F. ) ;
#10487 = CARTESIAN_POINT ( 'NONE',  ( -40.00000000000000000, 68.00000000000000000, 26.00000000000000355 ) ) ;
#10488 = DIRECTION ( 'NONE',  ( 0.000000000000000000, 0.000000000000000000, -1.000000000000000000 ) ) ;
#10489 = DIRECTION ( 'NONE',  ( -0.000000000000000000, -1.000000000000000000, -0.000000000000000000 ) ) ;
#10490 = CIRCLE ( 'NONE', #1584, 4.999999999999997335 ) ;
#10491 =( NAMED_UNIT ( * ) PLANE_ANGLE_UNIT ( ) SI_UNIT ( $, .RADIAN. ) );
#10492 = AXIS2_PLACEMENT_3D ( 'NONE', #19224, #6668, #6459 ) ;
#10493 = CARTESIAN_POINT ( 'NONE',  ( -37.00000000000000000, 0.000000000000000000, -22.99999999999999645 ) ) ;
#10494 = LINE ( 'NONE', #9063, #7787 ) ;
#10495 = DIRECTION ( 'NONE',  ( 0.000000000000000000, 0.000000000000000000, 1.000000000000000000 ) ) ;
#10496 = FACE_OUTER_BOUND ( 'NONE', #11534, .T. ) ;
#10497 = CARTESIAN_POINT ( 'NONE',  ( 111.4893729001366012, 129.7247684487574588, 281.6050404526570219 ) ) ;
#10498 =( LENGTH_UNIT ( ) NAMED_UNIT ( * ) SI_UNIT ( .MILLI., .METRE. ) );
#10499 = ADVANCED_FACE ( 'NONE', ( #6843 ), #6631, .T. ) ;
#10500 =( NAMED_UNIT ( * ) SI_UNIT ( $, .STERADIAN. ) SOLID_ANGLE_UNIT ( ) );
#10501 = CYLINDRICAL_SURFACE ( 'NONE', #20062, 10.00000000000000888 ) ;
#10502 = SURFACE_SIDE_STYLE ('',( #10197 ) ) ;
#10503 = CARTESIAN_POINT ( 'NONE',  ( 40.00000000000000711, 0.000000000000000000, -34.99999999999997868 ) ) ;
#10504 = DIRECTION ( 'NONE',  ( -1.000000000000000000, -0.000000000000000000, -0.000000000000000000 ) ) ;
#10505 = VECTOR ( 'NONE', #6715, 1000.000000000000000 ) ;
#10506 = EDGE_CURVE ( 'NONE', #4609, #17030, #10019, .T. ) ;
#10507 = CIRCLE ( 'NONE', #2918, 3.299999999999997158 ) ;
#10508 = COLOUR_RGB ( '', 0.31764706, 0.68627451, 0.89019608) ;
#10509 = ORIENTED_EDGE ( 'NONE', *, *, #15577, .F. ) ;
#10510 = VERTEX_POINT ( 'NONE', #5190 ) ;
#10511 = ORIENTED_EDGE ( 'NONE', *, *, #2027, .T. ) ;
#10512 = ADVANCED_FACE ( 'NONE', ( #19377 ), #1954, .T. ) ;
#10513 = SURFACE_STYLE_FILL_AREA ( #828 ) ;
#10514 = EDGE_LOOP ( 'NONE', ( #17641, #18518, #6294, #15082, #4487, #10697 ) ) ;
#10515 = VERTEX_POINT ( 'NONE', #424 ) ;
#10516 = CARTESIAN_POINT ( 'NONE',  ( -22.99999999999999645, 68.00000000000000000, -36.99999999999999289 ) ) ;
#10517 = ADVANCED_FACE ( 'NONE', ( #16334 ), #6742, .F. ) ;
#10518 = DIRECTION ( 'NONE',  ( -1.000000000000000000, 0.000000000000000000, 0.000000000000000000 ) ) ;
#10519 = UNCERTAINTY_MEASURE_WITH_UNIT (LENGTH_MEASURE( 1.000000000000000082E-05 ), #8571, 'distance_accuracy_value', 'NONE');
#10520 = CARTESIAN_POINT ( 'NONE',  ( 31.00000000000002842, 68.00000000000000000, 23.00000000000001066 ) ) ;
#10521 = APPLICATION_CONTEXT ( 'automotive_design' ) ;
#10522 =( GEOMETRIC_REPRESENTATION_CONTEXT ( 3 ) GLOBAL_UNCERTAINTY_ASSIGNED_CONTEXT ( ( #16514 ) ) GLOBAL_UNIT_ASSIGNED_CONTEXT ( ( #11193, #3264, #6468 ) ) REPRESENTATION_CONTEXT ( 'NONE', 'WORKASPACE' ) );
#10523 = EDGE_CURVE ( 'NONE', #8826, #8340, #2168, .T. ) ;
#10524 = SURFACE_SIDE_STYLE ('',( #13814 ) ) ;
#10525 = VECTOR ( 'NONE', #18491, 1000.000000000000000 ) ;
#10526 = VECTOR ( 'NONE', #17559, 1000.000000000000000 ) ;
#10527 = ADVANCED_FACE ( 'NONE', ( #11460 ), #9915, .F. ) ;
#10528 = DIRECTION ( 'NONE',  ( -0.000000000000000000, 1.000000000000000000, -0.000000000000000000 ) ) ;
#10529 = LINE ( 'NONE', #20092, #19858 ) ;
#10530 = CARTESIAN_POINT ( 'NONE',  ( -211.5106270998635409, 113.1299228374912502, 220.6387154965113382 ) ) ;
#10531 = FACE_OUTER_BOUND ( 'NONE', #2621, .T. ) ;
#10532 = PLANE ( 'NONE',  #11941 ) ;
#10533 = EDGE_LOOP ( 'NONE', ( #8246, #11388 ) ) ;
#10534 =( NAMED_UNIT ( * ) SI_UNIT ( $, .STERADIAN. ) SOLID_ANGLE_UNIT ( ) );
#10535 = SURFACE_SIDE_STYLE ('',( #4256 ) ) ;
#10536 = VECTOR ( 'NONE', #19703, 1000.000000000000000 ) ;
#10537 = CIRCLE ( 'NONE', #5283, 2.000000000000001776 ) ;
#10538 = ORIENTED_EDGE ( 'NONE', *, *, #9162, .F. ) ;
#10539 = UNCERTAINTY_MEASURE_WITH_UNIT (LENGTH_MEASURE( 1.000000000000000082E-05 ), #2320, 'distance_accuracy_value', 'NONE');
#10540 = ORIENTED_EDGE ( 'NONE', *, *, #4493, .T. ) ;
#10541 = EDGE_CURVE ( 'NONE', #17811, #5524, #1092, .T. ) ;
#10542 = SURFACE_STYLE_FILL_AREA ( #4265 ) ;
#10543 = UNCERTAINTY_MEASURE_WITH_UNIT (LENGTH_MEASURE( 1.000000000000000082E-05 ), #9171, 'distance_accuracy_value', 'NONE');
#10544 = VERTEX_POINT ( 'NONE', #7426 ) ;
#10545 = DIRECTION ( 'NONE',  ( 1.000000000000000000, 0.000000000000000000, 0.000000000000000000 ) ) ;
#10546 = SURFACE_STYLE_FILL_AREA ( #15300 ) ;
#10547 = PRESENTATION_STYLE_ASSIGNMENT (( #10645 ) ) ;
#10548 = EDGE_CURVE ( 'NONE', #18451, #5238, #13706, .T. ) ;
#10549 = AXIS2_PLACEMENT_3D ( 'NONE', #4324, #2563, #4426 ) ;
#10550 = ADVANCED_FACE ( 'NONE', ( #4227 ), #19961, .F. ) ;
#10551 = CARTESIAN_POINT ( 'NONE',  ( -80.06977618402036967, 141.0668072968081503, 501.4424506789935094 ) ) ;
#10552 = DIRECTION ( 'NONE',  ( -0.000000000000000000, 1.000000000000000000, -0.000000000000000000 ) ) ;
#10553 = CIRCLE ( 'NONE', #2295, 4.000000000000000000 ) ;
#10554 = CARTESIAN_POINT ( 'NONE',  ( 35.99999999999999289, 10.00000000000000000, 21.99999999999999645 ) ) ;
#10555 = ORIENTED_EDGE ( 'NONE', *, *, #13493, .F. ) ;
#10556 = CARTESIAN_POINT ( 'NONE',  ( 0.000000000000000000, 65.20000000000000284, -5.741599279633704455E-16 ) ) ;
#10557 = FACE_BOUND ( 'NONE', #17671, .T. ) ;
#10558 = DIRECTION ( 'NONE',  ( 0.000000000000000000, 1.000000000000000000, 0.000000000000000000 ) ) ;
#10559 = PRODUCT_CONTEXT ( 'NONE', #11576, 'mechanical' ) ;
#10560 = EDGE_LOOP ( 'NONE', ( #8911, #7084, #1125, #6984, #694, #18891 ) ) ;
#10561 = VECTOR ( 'NONE', #15253, 1000.000000000000000 ) ;
#10562 = ORIENTED_EDGE ( 'NONE', *, *, #6463, .F. ) ;
#10563 = ORIENTED_EDGE ( 'NONE', *, *, #598, .F. ) ;
#10564 = ORIENTED_EDGE ( 'NONE', *, *, #16210, .F. ) ;
#10565 = CIRCLE ( 'NONE', #1647, 3.299999999999997158 ) ;
#10566 = VECTOR ( 'NONE', #11146, 1000.000000000000000 ) ;
#10567 = DIRECTION ( 'NONE',  ( -1.000000000000000000, 0.000000000000000000, 0.000000000000000000 ) ) ;
#10568 = ORIENTED_EDGE ( 'NONE', *, *, #10117, .T. ) ;
#10569 = CARTESIAN_POINT ( 'NONE',  ( 55.98937290013660117, 144.5787140289007198, 293.4524157190248275 ) ) ;
#10570 = ORIENTED_EDGE ( 'NONE', *, *, #15686, .F. ) ;
#10571 = DIRECTION ( 'NONE',  ( -7.715811803773179210E-14, 0.000000000000000000, -1.000000000000000000 ) ) ;
#10572 = EDGE_CURVE ( 'NONE', #2877, #16599, #13888, .T. ) ;
#10573 = CARTESIAN_POINT ( 'NONE',  ( 109.4893729001366012, 127.7247684487574588, 368.0000000000000000 ) ) ;
#10574 = CARTESIAN_POINT ( 'NONE',  ( 10.00000000000000000, 306.0487089519837127, -150.0000000000038369 ) ) ;
#10575 = FACE_BOUND ( 'NONE', #9815, .T. ) ;
#10576 = LINE ( 'NONE', #19832, #19213 ) ;
#10577 = LINE ( 'NONE', #8835, #7185 ) ;
#10578 = CARTESIAN_POINT ( 'NONE',  ( 0.000000000000000000, 316.7545334744432921, 205.1946179577815883 ) ) ;
#10579 = CARTESIAN_POINT ( 'NONE',  ( 493.8117674897343363, 134.2156642432025251, 245.0000000000000000 ) ) ;
#10580 = SHAPE_REPRESENTATION_RELATIONSHIP ( 'NONE' , 'NONE' ,  #7605, #9359 ) ;
#10581 = CARTESIAN_POINT ( 'NONE',  ( 35.00000000000000711, 0.000000000000000000, -35.00000000000000711 ) ) ;
#10582 = FILL_AREA_STYLE ('',( #18402 ) ) ;
#10583 = FILL_AREA_STYLE_COLOUR ( '', #20101 ) ;
#10584 = AXIS2_PLACEMENT_3D ( 'NONE', #15444, #3268, #7709 ) ;
#10585 = EDGE_LOOP ( 'NONE', ( #7730, #1135, #1301, #15370 ) ) ;
#10586 = EDGE_LOOP ( 'NONE', ( #15996, #9213 ) ) ;
#10587 = ORIENTED_EDGE ( 'NONE', *, *, #14645, .F. ) ;
#10588 = DIRECTION ( 'NONE',  ( 0.000000000000000000, 1.000000000000000000, -0.000000000000000000 ) ) ;
#10589 = VERTEX_POINT ( 'NONE', #12361 ) ;
#10590 = CARTESIAN_POINT ( 'NONE',  ( 503.8334540492693918, 191.8198460455371333, 225.0057801310552463 ) ) ;
#10591 = DIRECTION ( 'NONE',  ( -1.000000000000000000, -1.595148023886719315E-16, 0.000000000000000000 ) ) ;
#10592 = DIRECTION ( 'NONE',  ( 0.000000000000000000, -0.000000000000000000, 1.000000000000000000 ) ) ;
#10593 = ORIENTED_EDGE ( 'NONE', *, *, #14538, .F. ) ;
#10594 = CARTESIAN_POINT ( 'NONE',  ( 1.163414459189985485E-15, 10.00000000000000000, 9.500000000000000000 ) ) ;
#10595 = DIRECTION ( 'NONE',  ( 0.000000000000000000, 0.000000000000000000, -1.000000000000000000 ) ) ;
#10596 = DIRECTION ( 'NONE',  ( 0.000000000000000000, 1.000000000000000000, 0.000000000000000000 ) ) ;
#10597 = CARTESIAN_POINT ( 'NONE',  ( -211.5106270998635409, 103.1299228374912360, 29.36128450348865471 ) ) ;
#10598 = FILL_AREA_STYLE ('',( #19862 ) ) ;
#10599 = MECHANICAL_DESIGN_GEOMETRIC_PRESENTATION_REPRESENTATION (  '', ( #6344 ), #4352 ) ;
#10600 = DIRECTION ( 'NONE',  ( -1.000000000000000000, -0.000000000000000000, -0.000000000000000000 ) ) ;
#10601 = FACE_OUTER_BOUND ( 'NONE', #11076, .T. ) ;
#10602 = CARTESIAN_POINT ( 'NONE',  ( 153.4893729001366864, 103.1299228374914492, 29.36128450348865471 ) ) ;
#10603 = DIRECTION ( 'NONE',  ( 1.000000000000000000, 0.000000000000000000, 0.000000000000000000 ) ) ;
#10604 = PRESENTATION_STYLE_ASSIGNMENT (( #13796 ) ) ;
#10605 = PRESENTATION_LAYER_ASSIGNMENT (  '', '', ( #19469 ) ) ;
#10606 = VECTOR ( 'NONE', #8820, 1000.000000000000000 ) ;
#10607 = EDGE_CURVE ( 'NONE', #19010, #688, #16797, .T. ) ;
#10608 = EDGE_LOOP ( 'NONE', ( #12407, #17617, #18574, #7385 ) ) ;
#10609 = ORIENTED_EDGE ( 'NONE', *, *, #17417, .F. ) ;
#10610 = PRODUCT_DEFINITION_FORMATION_WITH_SPECIFIED_SOURCE ( 'ANY', '', #1497, .NOT_KNOWN. ) ;
#10611 = VECTOR ( 'NONE', #11878, 1000.000000000000000 ) ;
#10612 = FACE_BOUND ( 'NONE', #248, .T. ) ;
#10613 = VERTEX_POINT ( 'NONE', #12243 ) ;
#10614 = AXIS2_PLACEMENT_3D ( 'NONE', #7544, #16828, #5995 ) ;
#10615 = ORIENTED_EDGE ( 'NONE', *, *, #7811, .F. ) ;
#10616 = DIRECTION ( 'NONE',  ( 0.000000000000000000, 0.000000000000000000, -1.000000000000000000 ) ) ;
#10617 = LINE ( 'NONE', #20083, #759 ) ;
#10618 = FACE_OUTER_BOUND ( 'NONE', #15233, .T. ) ;
#10619 = VECTOR ( 'NONE', #19835, 1000.000000000000000 ) ;
#10620 = DIRECTION ( 'NONE',  ( 0.000000000000000000, 1.000000000000000000, 0.000000000000000000 ) ) ;
#10621 = SURFACE_STYLE_USAGE ( .BOTH. , #7540 ) ;
#10622 = EDGE_CURVE ( 'NONE', #15498, #10365, #20059, .T. ) ;
#10623 = CIRCLE ( 'NONE', #1722, 10.00000000000000888 ) ;
#10624 = DIRECTION ( 'NONE',  ( -0.000000000000000000, -1.000000000000000000, -0.000000000000000000 ) ) ;
#10625 = DIRECTION ( 'NONE',  ( 0.000000000000000000, 1.000000000000000000, 0.000000000000000000 ) ) ;
#10626 = DIRECTION ( 'NONE',  ( 0.000000000000000000, 0.000000000000000000, -1.000000000000000000 ) ) ;
#10627 = CARTESIAN_POINT ( 'NONE',  ( -79.66506982498428613, 138.8257004745550773, 489.9345105970523946 ) ) ;
#10628 = COLOUR_RGB ( '', 0.72549020, 0.75294118, 0.79215686) ;
#10629 = EDGE_CURVE ( 'NONE', #2872, #12998, #14098, .T. ) ;
#10630 = ORIENTED_EDGE ( 'NONE', *, *, #18406, .F. ) ;
#10631 = CYLINDRICAL_SURFACE ( 'NONE', #3918, 5.000000000000000888 ) ;
#10632 =( NAMED_UNIT ( * ) PLANE_ANGLE_UNIT ( ) SI_UNIT ( $, .RADIAN. ) );
#10633 = LINE ( 'NONE', #1019, #17582 ) ;
#10634 = EDGE_CURVE ( 'NONE', #5440, #19306, #12678, .T. ) ;
#10635 = VECTOR ( 'NONE', #16114, 1000.000000000000000 ) ;
#10636 = EDGE_CURVE ( 'NONE', #10482, #3302, #13353, .T. ) ;
#10637 = ORIENTED_EDGE ( 'NONE', *, *, #2695, .T. ) ;
#10638 = CIRCLE ( 'NONE', #432, 10.00000000000000888 ) ;
#10639 = ORIENTED_EDGE ( 'NONE', *, *, #13428, .T. ) ;
#10640 = CIRCLE ( 'NONE', #18531, 5.000000000000000888 ) ;
#10641 = CARTESIAN_POINT ( 'NONE',  ( 108.9893729001365870, 108.8727366810872468, 338.2196854716659118 ) ) ;
#10642 = DIRECTION ( 'NONE',  ( 1.000000000000000000, 0.000000000000000000, 0.000000000000000000 ) ) ;
#10643 = CARTESIAN_POINT ( 'NONE',  ( 498.8117674897343932, 191.8198460455371333, 168.2339398819845826 ) ) ;
#10644 = LINE ( 'NONE', #5603, #10002 ) ;
#10646 = EDGE_CURVE ( 'NONE', #12110, #9346, #19899, .T. ) ;
#10645 = SURFACE_STYLE_USAGE ( .BOTH. , #5707 ) ;
#10647 = VECTOR ( 'NONE', #12644, 1000.000000000000000 ) ;
#10648 = DIRECTION ( 'NONE',  ( -0.000000000000000000, 1.000000000000000000, -0.000000000000000000 ) ) ;
#10649 = SURFACE_SIDE_STYLE ('',( #18369 ) ) ;
#10650 = ORIENTED_EDGE ( 'NONE', *, *, #17038, .T. ) ;
#10651 = DIRECTION ( 'NONE',  ( 1.000000000000000000, 5.889072920838430686E-16, -0.000000000000000000 ) ) ;
#10652 = ORIENTED_EDGE ( 'NONE', *, *, #6604, .F. ) ;
#10653 = FACE_OUTER_BOUND ( 'NONE', #18360, .T. ) ;
#10654 = SHAPE_DEFINITION_REPRESENTATION ( #20088, #10923 ) ;
#10655 = EDGE_CURVE ( 'NONE', #12344, #10821, #3469, .T. ) ;
#10656 = COLOUR_RGB ( '', 0.31764706, 0.68627451, 0.89019608) ;
#10657 = ORIENTED_EDGE ( 'NONE', *, *, #2864, .T. ) ;
#10658 = DIRECTION ( 'NONE',  ( 0.000000000000000000, -1.000000000000000000, 0.000000000000000000 ) ) ;
#10659 = ORIENTED_EDGE ( 'NONE', *, *, #5858, .T. ) ;
#10660 = AXIS2_PLACEMENT_3D ( 'NONE', #9126, #13759, #1056 ) ;
#10661 = ADVANCED_FACE ( 'NONE', ( #6184 ), #13657, .T. ) ;
#10662 = ORIENTED_EDGE ( 'NONE', *, *, #3857, .F. ) ;
#10663 = ORIENTED_EDGE ( 'NONE', *, *, #2982, .T. ) ;
#10664 = VECTOR ( 'NONE', #1680, 1000.000000000000000 ) ;
#10665 =( GEOMETRIC_REPRESENTATION_CONTEXT ( 3 ) GLOBAL_UNCERTAINTY_ASSIGNED_CONTEXT ( ( #18342 ) ) GLOBAL_UNIT_ASSIGNED_CONTEXT ( ( #18048, #11376, #8395 ) ) REPRESENTATION_CONTEXT ( 'NONE', 'WORKASPACE' ) );
#10666 = COLOUR_RGB ( '', 0.40784314, 0.44705882, 0.49803922) ;
#10667 = LINE ( 'NONE', #10465, #20252 ) ;
#10668 = VERTEX_POINT ( 'NONE', #10913 ) ;
#10669 = CARTESIAN_POINT ( 'NONE',  ( 0.2320613958866641346, 140.7529646695461736, 501.1799789315547287 ) ) ;
#10670 = EDGE_LOOP ( 'NONE', ( #8510, #12913, #6802, #16745 ) ) ;
#10671 = DIRECTION ( 'NONE',  ( 6.123031769111888756E-17, 0.000000000000000000, 1.000000000000000000 ) ) ;
#10672 = CIRCLE ( 'NONE', #9023, 10.00000000000000888 ) ;
#10673 = CARTESIAN_POINT ( 'NONE',  ( -41.50085094405407915, 175.4489062796178871, 505.3921618609452935 ) ) ;
#10674 = AXIS2_PLACEMENT_3D ( 'NONE', #16223, #18418, #5966 ) ;
#10675 = DIRECTION ( 'NONE',  ( -1.000000000000000000, -0.000000000000000000, -0.000000000000000000 ) ) ;
#10676 = DIRECTION ( 'NONE',  ( 1.000000000000000000, -0.000000000000000000, 0.000000000000000000 ) ) ;
#10677 = LINE ( 'NONE', #15538, #15795 ) ;
#10678 = PRESENTATION_STYLE_ASSIGNMENT (( #4812 ) ) ;
#10679 = EDGE_CURVE ( 'NONE', #951, #2425, #20236, .T. ) ;
#10680 = DIRECTION ( 'NONE',  ( 0.000000000000000000, 0.000000000000000000, 1.000000000000000000 ) ) ;
#10681 =( GEOMETRIC_REPRESENTATION_CONTEXT ( 3 ) GLOBAL_UNCERTAINTY_ASSIGNED_CONTEXT ( ( #2058 ) ) GLOBAL_UNIT_ASSIGNED_CONTEXT ( ( #8285, #14360, #17539 ) ) REPRESENTATION_CONTEXT ( 'NONE', 'WORKASPACE' ) );
#10682 = CIRCLE ( 'NONE', #6421, 34.00000000000000000 ) ;
#10683 = DIRECTION ( 'NONE',  ( 1.000000000000000000, 0.000000000000000000, -0.000000000000000000 ) ) ;
#10684 = FACE_OUTER_BOUND ( 'NONE', #18471, .T. ) ;
#10685 = CARTESIAN_POINT ( 'NONE',  ( 30.90550859392620353, -45.11391548236647253, 66.87703344121217697 ) ) ;
#10687 = AXIS2_PLACEMENT_3D ( 'NONE', #6830, #13120, #3721 ) ;
#10686 = FACE_OUTER_BOUND ( 'NONE', #11100, .T. ) ;
#10688 = AXIS2_PLACEMENT_3D ( 'NONE', #17827, #17931, #11451 ) ;
#10689 =( NAMED_UNIT ( * ) SI_UNIT ( $, .STERADIAN. ) SOLID_ANGLE_UNIT ( ) );
#10690 = DIRECTION ( 'NONE',  ( 0.000000000000000000, 0.000000000000000000, -1.000000000000000000 ) ) ;
#10691 = ORIENTED_EDGE ( 'NONE', *, *, #15964, .T. ) ;
#10692 =( GEOMETRIC_REPRESENTATION_CONTEXT ( 3 ) GLOBAL_UNCERTAINTY_ASSIGNED_CONTEXT ( ( #5192 ) ) GLOBAL_UNIT_ASSIGNED_CONTEXT ( ( #13425, #11868, #16811 ) ) REPRESENTATION_CONTEXT ( 'NONE', 'WORKASPACE' ) );
#10693 = VECTOR ( 'NONE', #10671, 1000.000000000000000 ) ;
#10694 = ORIENTED_EDGE ( 'NONE', *, *, #19971, .F. ) ;
#10695 = AXIS2_PLACEMENT_3D ( 'NONE', #12148, #10596, #15562 ) ;
#10696 = ORIENTED_EDGE ( 'NONE', *, *, #13145, .F. ) ;
#10697 = ORIENTED_EDGE ( 'NONE', *, *, #2906, .T. ) ;
#10698 = PRESENTATION_LAYER_ASSIGNMENT (  '', '', ( #13997 ) ) ;
#10699 = DIRECTION ( 'NONE',  ( 1.000000000000000000, 0.000000000000000000, -0.000000000000000000 ) ) ;
#10700 = PRESENTATION_LAYER_ASSIGNMENT (  '', '', ( #8723 ) ) ;
#10701 = ORIENTED_EDGE ( 'NONE', *, *, #12318, .T. ) ;
#10702 = DIRECTION ( 'NONE',  ( 0.000000000000000000, 0.000000000000000000, -1.000000000000000000 ) ) ;
#10703 = AXIS2_PLACEMENT_3D ( 'NONE', #9844, #8306, #14579 ) ;
#10704 = FACE_OUTER_BOUND ( 'NONE', #14078, .T. ) ;
#10705 = ORIENTED_EDGE ( 'NONE', *, *, #3467, .T. ) ;
#10706 = PRESENTATION_STYLE_ASSIGNMENT (( #4416 ) ) ;
#10707 = FILL_AREA_STYLE_COLOUR ( '', #5813 ) ;
#10708 = VECTOR ( 'NONE', #9500, 1000.000000000000000 ) ;
#10709 = DIRECTION ( 'NONE',  ( 0.000000000000000000, -0.6449357872488920007, -0.7642367632649269549 ) ) ;
#10710 = FACE_OUTER_BOUND ( 'NONE', #11770, .T. ) ;
#10711 = LINE ( 'NONE', #12069, #18667 ) ;
#10712 = VECTOR ( 'NONE', #12741, 1000.000000000000000 ) ;
#10713 = SURFACE_STYLE_FILL_AREA ( #990 ) ;
#10714 = DIRECTION ( 'NONE',  ( 0.000000000000000000, 0.000000000000000000, -1.000000000000000000 ) ) ;
#10715 = LINE ( 'NONE', #9637, #20099 ) ;
#10716 = CYLINDRICAL_SURFACE ( 'NONE', #16143, 10.00000000000000888 ) ;
#10717 = ADVANCED_FACE ( 'NONE', ( #9157 ), #18326, .T. ) ;
#10718 = ORIENTED_EDGE ( 'NONE', *, *, #13370, .T. ) ;
#10719 = EDGE_LOOP ( 'NONE', ( #1789, #20048, #9881 ) ) ;
#10720 = EDGE_LOOP ( 'NONE', ( #1564, #16242, #11586, #8432 ) ) ;
#10721 = MECHANICAL_DESIGN_GEOMETRIC_PRESENTATION_REPRESENTATION (  '', ( #16023 ), #3830 ) ;
#10722 = DIRECTION ( 'NONE',  ( 0.000000000000000000, 1.000000000000000000, 0.000000000000000000 ) ) ;
#10723 = ORIENTED_EDGE ( 'NONE', *, *, #3718, .T. ) ;
#10724 = VERTEX_POINT ( 'NONE', #15456 ) ;
#10725 = PLANE ( 'NONE',  #9411 ) ;
#10726 = VECTOR ( 'NONE', #9082, 1000.000000000000000 ) ;
#10727 = PLANE ( 'NONE',  #18530 ) ;
#10728 = UNCERTAINTY_MEASURE_WITH_UNIT (LENGTH_MEASURE( 1.000000000000000082E-05 ), #4843, 'distance_accuracy_value', 'NONE');
#10729 = DIRECTION ( 'NONE',  ( 0.000000000000000000, -0.7071067811865336949, 0.7071067811865614505 ) ) ;
#10730 = DIRECTION ( 'NONE',  ( 1.000000000000000000, -0.000000000000000000, 0.000000000000000000 ) ) ;
#10731 = PRODUCT_DEFINITION_SHAPE ( 'NONE', 'NONE',  #1129 ) ;
#10732 = DIRECTION ( 'NONE',  ( 0.000000000000000000, 1.000000000000000000, 0.000000000000000000 ) ) ;
#10733 = DIRECTION ( 'NONE',  ( 1.000000000000000000, -0.000000000000000000, 4.956352788505159323E-16 ) ) ;
#10734 = EDGE_CURVE ( 'NONE', #11175, #13635, #10807, .T. ) ;
#10735 = CARTESIAN_POINT ( 'NONE',  ( -20.00000000000003197, 3.000000000000000000, 37.00000000000000711 ) ) ;
#10736 = FACE_OUTER_BOUND ( 'NONE', #15151, .T. ) ;
#10737 = CARTESIAN_POINT ( 'NONE',  ( -0.4453075966856865908, 139.8159989653383661, 500.9064470951030330 ) ) ;
#10738 = ORIENTED_EDGE ( 'NONE', *, *, #2801, .F. ) ;
#10739 = LINE ( 'NONE', #12394, #18562 ) ;
#10740 =( NAMED_UNIT ( * ) SI_UNIT ( $, .STERADIAN. ) SOLID_ANGLE_UNIT ( ) );
#10741 = COLOUR_RGB ( '', 0.31764706, 0.68627451, 0.89019608) ;
#10742 = EDGE_CURVE ( 'NONE', #12019, #13739, #9363, .T. ) ;
#10743 = ORIENTED_EDGE ( 'NONE', *, *, #11599, .T. ) ;
#10744 = EDGE_CURVE ( 'NONE', #7792, #17989, #12345, .T. ) ;
#10745 = ORIENTED_EDGE ( 'NONE', *, *, #20075, .T. ) ;
#10746 = CARTESIAN_POINT ( 'NONE',  ( 10.00000000000000000, 309.2289037985885898, -86.48019484660916589 ) ) ;
#10747 = DIRECTION ( 'NONE',  ( 0.000000000000000000, -1.000000000000000000, 0.000000000000000000 ) ) ;
#10748 = ORIENTED_EDGE ( 'NONE', *, *, #4339, .T. ) ;
#10749 = FILL_AREA_STYLE ('',( #4566 ) ) ;
#10750 = SURFACE_STYLE_USAGE ( .BOTH. , #2607 ) ;
#10751 = EDGE_CURVE ( 'NONE', #9454, #17589, #19019, .T. ) ;
#10752 = CARTESIAN_POINT ( 'NONE',  ( -78.99999999999995737, 139.2066006846527841, 488.2525619656395861 ) ) ;
#10753 = FACE_OUTER_BOUND ( 'NONE', #3218, .T. ) ;
#10754 = CARTESIAN_POINT ( 'NONE',  ( -25.99999999999999645, 0.000000000000000000, 40.00000000000002132 ) ) ;
#10755 =( LENGTH_UNIT ( ) NAMED_UNIT ( * ) SI_UNIT ( .MILLI., .METRE. ) );
#10756 = ORIENTED_EDGE ( 'NONE', *, *, #11655, .T. ) ;
#10757 = CARTESIAN_POINT ( 'NONE',  ( -31.81980515339462912, 11.00000000000000000, 31.81980515339465043 ) ) ;
#10758 = EDGE_CURVE ( 'NONE', #18212, #4662, #17603, .T. ) ;
#10759 = VERTEX_POINT ( 'NONE', #8231 ) ;
#10760 = CARTESIAN_POINT ( 'NONE',  ( 54.31780002488278569, 211.0574367717017594, 346.4752554294134939 ) ) ;
#10761 = CARTESIAN_POINT ( 'NONE',  ( 35.00000000000000711, 8.000000000000000000, -35.00000000000000711 ) ) ;
#10762 = PRODUCT_CONTEXT ( 'NONE', #6316, 'mechanical' ) ;
#10763 = ORIENTED_EDGE ( 'NONE', *, *, #10548, .F. ) ;
#10764 = ORIENTED_EDGE ( 'NONE', *, *, #19739, .T. ) ;
#10765 = FACE_OUTER_BOUND ( 'NONE', #8937, .T. ) ;
#10766 = ORIENTED_EDGE ( 'NONE', *, *, #10924, .F. ) ;
#10767 = ORIENTED_EDGE ( 'NONE', *, *, #672, .F. ) ;
#10768 = ADVANCED_FACE ( 'NONE', ( #11205, #17701, #15989, #4931, #17390 ), #6482, .F. ) ;
#10769 = ORIENTED_EDGE ( 'NONE', *, *, #7862, .F. ) ;
#10770 = PLANE ( 'NONE',  #8752 ) ;
#10771 = VERTEX_POINT ( 'NONE', #6690 ) ;
#10772 = LINE ( 'NONE', #17061, #218 ) ;
#10773 = ORIENTED_EDGE ( 'NONE', *, *, #9046, .F. ) ;
#10774 = ADVANCED_FACE ( 'NONE', ( #14196, #12982 ), #18933, .T. ) ;
#10775 = CARTESIAN_POINT ( 'NONE',  ( -1.242741617435013737E-14, 216.7545334744432921, 501.8237260975781737 ) ) ;
#10776 = DIRECTION ( 'NONE',  ( -0.000000000000000000, -1.000000000000000000, 0.000000000000000000 ) ) ;
#10777 = CARTESIAN_POINT ( 'NONE',  ( 4.163799117101000559E-15, 16.00000000000000000, 34.00000000000000000 ) ) ;
#10778 = SURFACE_STYLE_USAGE ( .BOTH. , #15425 ) ;
#10779 = EDGE_CURVE ( 'NONE', #7206, #5094, #490, .T. ) ;
#10780 = DIRECTION ( 'NONE',  ( -0.000000000000000000, -0.000000000000000000, 1.000000000000000000 ) ) ;
#10781 = SURFACE_STYLE_USAGE ( .BOTH. , #13679 ) ;
#10782 =( LENGTH_UNIT ( ) NAMED_UNIT ( * ) SI_UNIT ( .MILLI., .METRE. ) );
#10783 = EDGE_CURVE ( 'NONE', #19735, #5835, #2141, .T. ) ;
#10784 = DIRECTION ( 'NONE',  ( -0.000000000000000000, -1.000000000000000000, -0.000000000000000000 ) ) ;
#10785 = PRESENTATION_STYLE_ASSIGNMENT (( #7895 ) ) ;
#10786 = CARTESIAN_POINT ( 'NONE',  ( 108.9893729001366154, 130.3113892758444194, 284.0770112900635809 ) ) ;
#10787 = DIRECTION ( 'NONE',  ( -0.6031630618355672269, -1.916859900655997964E-19, 0.7976179040349733462 ) ) ;
#10788 = CARTESIAN_POINT ( 'NONE',  ( 153.4893729001366864, 123.1299228374914634, 170.4174721992565082 ) ) ;
#10789 =( LENGTH_UNIT ( ) NAMED_UNIT ( * ) SI_UNIT ( .MILLI., .METRE. ) );
#10790 = LINE ( 'NONE', #465, #7306 ) ;
#10791 = SURFACE_SIDE_STYLE ('',( #4512 ) ) ;
#10792 = CIRCLE ( 'NONE', #14736, 10.00000000000000888 ) ;
#10793 = VERTEX_POINT ( 'NONE', #8520 ) ;
#10794 = VECTOR ( 'NONE', #5539, 1000.000000000000000 ) ;
#10795 = ORIENTED_EDGE ( 'NONE', *, *, #502, .T. ) ;
#10796 = VERTEX_POINT ( 'NONE', #5241 ) ;
#10797 = VERTEX_POINT ( 'NONE', #16577 ) ;
#10798 = PRESENTATION_STYLE_ASSIGNMENT (( #3371 ) ) ;
#10799 = SURFACE_STYLE_FILL_AREA ( #2756 ) ;
#10800 = ORIENTED_EDGE ( 'NONE', *, *, #17080, .T. ) ;
#10801 = CARTESIAN_POINT ( 'NONE',  ( 5.569974746830579804, 0.000000000000000000, 0.000000000000000000 ) ) ;
#10802 = CARTESIAN_POINT ( 'NONE',  ( -211.5106270998635409, 103.1299228374912360, 170.4174721992565082 ) ) ;
#10803 = ORIENTED_EDGE ( 'NONE', *, *, #17077, .T. ) ;
#10804 = ADVANCED_FACE ( 'NONE', ( #14916 ), #3398, .T. ) ;
#10805 = FACE_BOUND ( 'NONE', #7849, .T. ) ;
#10806 = DIRECTION ( 'NONE',  ( 0.000000000000000000, 0.000000000000000000, 1.000000000000000000 ) ) ;
#10807 = LINE ( 'NONE', #17087, #19267 ) ;
#10808 = AXIS2_PLACEMENT_3D ( 'NONE', #11494, #3571, #2408 ) ;
#10809 = CARTESIAN_POINT ( 'NONE',  ( -3.000000000000000000, -1.836909530733565148E-16, 3.000000000000000000 ) ) ;
#10810 = EDGE_CURVE ( 'NONE', #3271, #12099, #19528, .T. ) ;
#10811 = DIRECTION ( 'NONE',  ( 1.000000000000000000, 0.000000000000000000, 0.000000000000000000 ) ) ;
#10812 = DIRECTION ( 'NONE',  ( 1.450371633464475582E-15, 0.000000000000000000, 1.000000000000000000 ) ) ;
#10813 = SURFACE_SIDE_STYLE ('',( #6595 ) ) ;
#10814 = ORIENTED_EDGE ( 'NONE', *, *, #2943, .F. ) ;
#10815 = VERTEX_POINT ( 'NONE', #11732 ) ;
#10816 = ORIENTED_EDGE ( 'NONE', *, *, #19678, .F. ) ;
#10817 = ORIENTED_EDGE ( 'NONE', *, *, #9808, .F. ) ;
#10818 =( NAMED_UNIT ( * ) SI_UNIT ( $, .STERADIAN. ) SOLID_ANGLE_UNIT ( ) );
#10819 = VERTEX_POINT ( 'NONE', #11616 ) ;
#10820 = ORIENTED_EDGE ( 'NONE', *, *, #12156, .T. ) ;
#10821 = VERTEX_POINT ( 'NONE', #14808 ) ;
#10822 = FACE_OUTER_BOUND ( 'NONE', #16726, .T. ) ;
#10823 = SURFACE_STYLE_FILL_AREA ( #4543 ) ;
#10824 = CYLINDRICAL_SURFACE ( 'NONE', #5965, 14.59999999999999964 ) ;
#10825 = SURFACE_STYLE_FILL_AREA ( #1619 ) ;
#10826 = FACE_OUTER_BOUND ( 'NONE', #5232, .T. ) ;
#10827 = ORIENTED_EDGE ( 'NONE', *, *, #8661, .T. ) ;
#10828 = EDGE_CURVE ( 'NONE', #19038, #8344, #6991, .T. ) ;
#10829 = FILL_AREA_STYLE ('',( #14118 ) ) ;
#10830 = CARTESIAN_POINT ( 'NONE',  ( -26.00000000000002132, 10.00000000000000000, 40.00000000000000711 ) ) ;
#10831 = LINE ( 'NONE', #9395, #1436 ) ;
#10832 = AXIS2_PLACEMENT_3D ( 'NONE', #18245, #10620, #4157 ) ;
#10833 = LINE ( 'NONE', #8053, #16884 ) ;
#10834 = AXIS2_PLACEMENT_3D ( 'NONE', #9979, #8841, #5451 ) ;
#10835 = ORIENTED_EDGE ( 'NONE', *, *, #5848, .T. ) ;
#10836 =( GEOMETRIC_REPRESENTATION_CONTEXT ( 3 ) GLOBAL_UNCERTAINTY_ASSIGNED_CONTEXT ( ( #88 ) ) GLOBAL_UNIT_ASSIGNED_CONTEXT ( ( #2098, #2711, #1037 ) ) REPRESENTATION_CONTEXT ( 'NONE', 'WORKASPACE' ) );
#10837 = DIRECTION ( 'NONE',  ( 7.715811803773179210E-14, -0.000000000000000000, 1.000000000000000000 ) ) ;
#10838 = FACE_OUTER_BOUND ( 'NONE', #13883, .T. ) ;
#10839 = PLANE ( 'NONE',  #16623 ) ;
#10840 = VERTEX_POINT ( 'NONE', #7195 ) ;
#10841 = VECTOR ( 'NONE', #2645, 1000.000000000000000 ) ;
#10842 = ADVANCED_FACE ( 'NONE', ( #13392 ), #19630, .F. ) ;
#10843 = AXIS2_PLACEMENT_3D ( 'NONE', #17803, #10276, #15125 ) ;
#10844 = CARTESIAN_POINT ( 'NONE',  ( 30.99999999999997868, 10.00000000000000000, -30.99999999999999645 ) ) ;
#10845 = ORIENTED_EDGE ( 'NONE', *, *, #16596, .T. ) ;
#10846 = CARTESIAN_POINT ( 'NONE',  ( -36.00000000000000711, 10.00000000000000000, -19.00000000000000000 ) ) ;
#10847 = VERTEX_POINT ( 'NONE', #12215 ) ;
#10848 = SURFACE_STYLE_USAGE ( .BOTH. , #6127 ) ;
#10849 = LINE ( 'NONE', #20223, #17568 ) ;
#10850 = LINE ( 'NONE', #12721, #8071 ) ;
#10851 = CARTESIAN_POINT ( 'NONE',  ( -0.06844068954109454317, 140.2957399442693429, 501.7113191689081191 ) ) ;
#10852 = DIRECTION ( 'NONE',  ( -1.000000000000000000, -0.000000000000000000, -0.000000000000000000 ) ) ;
#10853 =( NAMED_UNIT ( * ) PLANE_ANGLE_UNIT ( ) SI_UNIT ( $, .RADIAN. ) );
#10854 = ADVANCED_FACE ( 'NONE', ( #7293 ), #4501, .F. ) ;
#10855 = DIRECTION ( 'NONE',  ( -0.000000000000000000, -1.000000000000000000, -0.000000000000000000 ) ) ;
#10856 = ORIENTED_EDGE ( 'NONE', *, *, #9072, .F. ) ;
#10857 = DIRECTION ( 'NONE',  ( 0.000000000000000000, 0.000000000000000000, 1.000000000000000000 ) ) ;
#10858 = CARTESIAN_POINT ( 'NONE',  ( 31.00000000000006395, 68.00000000000000000, -22.99999999999999289 ) ) ;
#10859 = SURFACE_STYLE_USAGE ( .BOTH. , #1657 ) ;
#10860 = VECTOR ( 'NONE', #2444, 1000.000000000000000 ) ;
#10861 = CIRCLE ( 'NONE', #13178, 0.9999999999999983347 ) ;
#10862 = PRESENTATION_LAYER_ASSIGNMENT (  '', '', ( #9545 ) ) ;
#10863 = VERTEX_POINT ( 'NONE', #15217 ) ;
#10864 = PRODUCT_RELATED_PRODUCT_CATEGORY ( 'part', '', ( #1497 ) ) ;
#10865 = DIRECTION ( 'NONE',  ( 0.000000000000000000, 0.000000000000000000, 1.000000000000000000 ) ) ;
#10866 = VERTEX_POINT ( 'NONE', #4204 ) ;
#10867 = EDGE_LOOP ( 'NONE', ( #9154, #3474, #16437, #2619 ) ) ;
#10868 = VERTEX_POINT ( 'NONE', #10473 ) ;
#10869 = EDGE_CURVE ( 'NONE', #9968, #5105, #7393, .T. ) ;
#10870 = PRESENTATION_STYLE_ASSIGNMENT (( #14068 ) ) ;
#10871 = VERTEX_POINT ( 'NONE', #2737 ) ;
#10872 = CARTESIAN_POINT ( 'NONE',  ( -2.959702524295976245E-14, 141.4901731731944210, 501.7345762936599272 ) ) ;
#10873 = VECTOR ( 'NONE', #2965, 1000.000000000000000 ) ;
#10874 = VECTOR ( 'NONE', #14268, 1000.000000000000000 ) ;
#10875 = DIRECTION ( 'NONE',  ( -1.135258727068398879E-15, 0.000000000000000000, 1.000000000000000000 ) ) ;
#10876 = AXIS2_PLACEMENT_3D ( 'NONE', #18350, #18450, #13730 ) ;
#10877 = LINE ( 'NONE', #11085, #7337 ) ;
#10878 = DIRECTION ( 'NONE',  ( -0.000000000000000000, -1.000000000000000000, -0.000000000000000000 ) ) ;
#10879 = LINE ( 'NONE', #1794, #14901 ) ;
#10881 = EDGE_CURVE ( 'NONE', #7735, #9619, #6160, .T. ) ;
#10880 = CARTESIAN_POINT ( 'NONE',  ( -20.99999999999999645, 19.00000000000000000, -31.00000000000003908 ) ) ;
#10882 = DIRECTION ( 'NONE',  ( 0.000000000000000000, -0.000000000000000000, 1.000000000000000000 ) ) ;
#10883 = ADVANCED_FACE ( 'NONE', ( #5938 ), #12328, .T. ) ;
#10884 = VERTEX_POINT ( 'NONE', #13868 ) ;
#10885 = LINE ( 'NONE', #20141, #17059 ) ;
#10886 = LINE ( 'NONE', #1363, #6005 ) ;
#10887 = DIRECTION ( 'NONE',  ( 0.000000000000000000, 0.000000000000000000, -1.000000000000000000 ) ) ;
#10888 =( NAMED_UNIT ( * ) SI_UNIT ( $, .STERADIAN. ) SOLID_ANGLE_UNIT ( ) );
#10889 =( NAMED_UNIT ( * ) SI_UNIT ( $, .STERADIAN. ) SOLID_ANGLE_UNIT ( ) );
#10890 = DIRECTION ( 'NONE',  ( -1.025567617263343161E-15, -0.7071067811865455743, -0.7071067811865493491 ) ) ;
#10891 = EDGE_CURVE ( 'NONE', #12591, #10263, #10677, .T. ) ;
#10892 = CARTESIAN_POINT ( 'NONE',  ( -34.99999999999996447, 0.000000000000000000, -40.00000000000000711 ) ) ;
#10893 = ORIENTED_EDGE ( 'NONE', *, *, #7353, .T. ) ;
#10894 = AXIS2_PLACEMENT_3D ( 'NONE', #438, #3331, #14558 ) ;
#10895 = EDGE_CURVE ( 'NONE', #10771, #18631, #3937, .T. ) ;
#10896 = VECTOR ( 'NONE', #913, 1000.000000000000000 ) ;
#10897 = ORIENTED_EDGE ( 'NONE', *, *, #2998, .T. ) ;
#10898 = EDGE_CURVE ( 'NONE', #7254, #15257, #3275, .T. ) ;
#10899 = ORIENTED_EDGE ( 'NONE', *, *, #2223, .T. ) ;
#10900 = PRODUCT ( 'HG-KN73JK', 'HG-KN73JK', '', ( #16959 ) ) ;
#10901 = ORIENTED_EDGE ( 'NONE', *, *, #12946, .F. ) ;
#10902 = PLANE ( 'NONE',  #4666 ) ;
#10903 = ADVANCED_FACE ( 'NONE', ( #12121, #18393, #4293, #10575, #1679 ), #5126, .F. ) ;
#10904 = CARTESIAN_POINT ( 'NONE',  ( -32.00000000000000711, 10.00000000000000000, -23.00000000000000000 ) ) ;
#10905 = ORIENTED_EDGE ( 'NONE', *, *, #5419, .T. ) ;
#10906 = CARTESIAN_POINT ( 'NONE',  ( -31.81980515339462912, 11.00000000000000000, -31.81980515339465043 ) ) ;
#10907 = LINE ( 'NONE', #8016, #5668 ) ;
#10908 = ORIENTED_EDGE ( 'NONE', *, *, #8167, .F. ) ;
#10909 = CARTESIAN_POINT ( 'NONE',  ( 498.8117674897343932, 134.2156642432025251, -2.775557561562891351E-14 ) ) ;
#10910 = TOROIDAL_SURFACE ( 'NONE', #2329, 8.000000000000000000, 1.000000000000000000 ) ;
#10911 = DIRECTION ( 'NONE',  ( 0.000000000000000000, 1.000000000000000000, 0.000000000000000000 ) ) ;
#10912 = VECTOR ( 'NONE', #13722, 1000.000000000000000 ) ;
#10913 = CARTESIAN_POINT ( 'NONE',  ( 10.00000000000000000, 341.0487089519837696, -133.5000000000032969 ) ) ;
#10914 = EDGE_CURVE ( 'NONE', #5827, #18716, #9519, .T. ) ;
#10915 = DIRECTION ( 'NONE',  ( 9.815121534730717399E-17, -1.000000000000000000, 0.000000000000000000 ) ) ;
#10916 =( NAMED_UNIT ( * ) SI_UNIT ( $, .STERADIAN. ) SOLID_ANGLE_UNIT ( ) );
#10917 = CARTESIAN_POINT ( 'NONE',  ( -81.18192946989245229, 138.7545334744432637, 491.0690926367356610 ) ) ;
#10918 = DIRECTION ( 'NONE',  ( 0.000000000000000000, 1.000000000000000000, 0.000000000000000000 ) ) ;
#10919 = DIRECTION ( 'NONE',  ( 0.000000000000000000, 0.000000000000000000, -1.000000000000000000 ) ) ;
#10920 = ORIENTED_EDGE ( 'NONE', *, *, #14532, .T. ) ;
#10921 = DIRECTION ( 'NONE',  ( 0.000000000000000000, 0.000000000000000000, -1.000000000000000000 ) ) ;
#10922 = APPLICATION_CONTEXT ( 'automotive_design' ) ;
#10923 = SHAPE_REPRESENTATION ( 'Part4', ( #2741 ), #19798 ) ;
#10924 = EDGE_CURVE ( 'NONE', #17380, #19179, #11170, .T. ) ;
#10925 = ORIENTED_EDGE ( 'NONE', *, *, #13826, .T. ) ;
#10926 = CIRCLE ( 'NONE', #7621, 4.999999999999997335 ) ;
#10927 = ORIENTED_EDGE ( 'NONE', *, *, #19777, .F. ) ;
#10928 = ORIENTED_EDGE ( 'NONE', *, *, #17469, .F. ) ;
#10929 = SURFACE_STYLE_FILL_AREA ( #3194 ) ;
#10930 = VECTOR ( 'NONE', #6576, 1000.000000000000000 ) ;
#10931 = VERTEX_POINT ( 'NONE', #3472 ) ;
#10932 = ORIENTED_EDGE ( 'NONE', *, *, #3201, .T. ) ;
#10933 = ORIENTED_EDGE ( 'NONE', *, *, #431, .F. ) ;
#10934 = LINE ( 'NONE', #6201, #18625 ) ;
#10935 = ADVANCED_FACE ( 'NONE', ( #17567 ), #7798, .F. ) ;
#10936 = DIRECTION ( 'NONE',  ( -0.000000000000000000, -1.000000000000000000, -0.000000000000000000 ) ) ;
#10937 = CARTESIAN_POINT ( 'NONE',  ( 53.48937290013658696, 103.1299228374913923, 170.4174721992565082 ) ) ;
#10938 = ORIENTED_EDGE ( 'NONE', *, *, #17810, .T. ) ;
#10939 = DIRECTION ( 'NONE',  ( 0.000000000000000000, 0.000000000000000000, -1.000000000000000000 ) ) ;
#10940 = DIRECTION ( 'NONE',  ( 1.000000000000000000, -0.000000000000000000, 0.000000000000000000 ) ) ;
#10941 = LINE ( 'NONE', #9280, #14303 ) ;
#10942 = DIRECTION ( 'NONE',  ( -1.000000000000000000, 0.000000000000000000, -0.000000000000000000 ) ) ;
#10943 = CARTESIAN_POINT ( 'NONE',  ( 0.6927201199992654157, 139.4947537936898243, 500.2388491393129470 ) ) ;
#10944 = ORIENTED_EDGE ( 'NONE', *, *, #19651, .T. ) ;
#10945 =( NAMED_UNIT ( * ) PLANE_ANGLE_UNIT ( ) SI_UNIT ( $, .RADIAN. ) );
#10946 = PRESENTATION_LAYER_ASSIGNMENT (  '', '', ( #2708 ) ) ;
#10947 = VERTEX_POINT ( 'NONE', #9529 ) ;
#10948 = AXIS2_PLACEMENT_3D ( 'NONE', #5044, #10173, #17610 ) ;
#10949 = CARTESIAN_POINT ( 'NONE',  ( -211.5106270998635409, 113.1299228374912502, 170.4174721992565082 ) ) ;
#10950 = CIRCLE ( 'NONE', #408, 5.000000000000000888 ) ;
#10951 = ORIENTED_EDGE ( 'NONE', *, *, #18093, .T. ) ;
#10952 = FACE_OUTER_BOUND ( 'NONE', #351, .T. ) ;
#10953 = DIRECTION ( 'NONE',  ( 0.000000000000000000, 1.000000000000000000, 0.000000000000000000 ) ) ;
#10954 = ORIENTED_EDGE ( 'NONE', *, *, #14519, .F. ) ;
#10955 =( NAMED_UNIT ( * ) PLANE_ANGLE_UNIT ( ) SI_UNIT ( $, .RADIAN. ) );
#10956 = LINE ( 'NONE', #15505, #773 ) ;
#10957 = AXIS2_PLACEMENT_3D ( 'NONE', #918, #19776, #19887 ) ;
#10958 = PLANE ( 'NONE',  #18266 ) ;
#10959 = CARTESIAN_POINT ( 'NONE',  ( 2.999999999999996003, 66.00000000000000000, 9.013878188659974811 ) ) ;
#10960 = CARTESIAN_POINT ( 'NONE',  ( -31.00000000000006750, 0.000000000000000000, 26.00000000000000355 ) ) ;
#10961 = FACE_OUTER_BOUND ( 'NONE', #15519, .T. ) ;
#10962 = VERTEX_POINT ( 'NONE', #14075 ) ;
#10963 = FACE_OUTER_BOUND ( 'NONE', #11814, .T. ) ;
#10964 = VECTOR ( 'NONE', #6566, 1000.000000000000000 ) ;
#10965 =( GEOMETRIC_REPRESENTATION_CONTEXT ( 3 ) GLOBAL_UNCERTAINTY_ASSIGNED_CONTEXT ( ( #12166 ) ) GLOBAL_UNIT_ASSIGNED_CONTEXT ( ( #17635, #9902, #17728 ) ) REPRESENTATION_CONTEXT ( 'NONE', 'WORKASPACE' ) );
#10966 = CARTESIAN_POINT ( 'NONE',  ( 31.00000000000001776, 10.00000000000000000, -25.99999999999999645 ) ) ;
#10967 = ORIENTED_EDGE ( 'NONE', *, *, #11137, .T. ) ;
#10968 = ORIENTED_EDGE ( 'NONE', *, *, #9786, .T. ) ;
#10969 = ORIENTED_EDGE ( 'NONE', *, *, #16834, .T. ) ;
#10970 = VERTEX_POINT ( 'NONE', #1575 ) ;
#10971 = ADVANCED_FACE ( 'NONE', ( #1796 ), #12959, .T. ) ;
#10972 = CIRCLE ( 'NONE', #8018, 2.000000000000001776 ) ;
#10973 = ORIENTED_EDGE ( 'NONE', *, *, #6801, .F. ) ;
#10974 = DIRECTION ( 'NONE',  ( 0.000000000000000000, 0.000000000000000000, 1.000000000000000000 ) ) ;
#10975 = ORIENTED_EDGE ( 'NONE', *, *, #1395, .F. ) ;
#10976 = AXIS2_PLACEMENT_3D ( 'NONE', #2033, #5175, #210 ) ;
#10977 = DIRECTION ( 'NONE',  ( 1.000000000000000000, 0.000000000000000000, -0.000000000000000000 ) ) ;
#10978 = ORIENTED_EDGE ( 'NONE', *, *, #2740, .T. ) ;
#10979 =( NAMED_UNIT ( * ) PLANE_ANGLE_UNIT ( ) SI_UNIT ( $, .RADIAN. ) );
#10980 = CARTESIAN_POINT ( 'NONE',  ( -22.99999999999999645, 68.00000000000000000, -36.99999999999999289 ) ) ;
#10981 = DIRECTION ( 'NONE',  ( -1.000000000000000000, 0.000000000000000000, 0.000000000000000000 ) ) ;
#10982 = EDGE_CURVE ( 'NONE', #14093, #10045, #10983, .T. ) ;
#10983 = LINE ( 'NONE', #17271, #8863 ) ;
#10984 = COLOUR_RGB ( '', 0.09019608, 0.27058824, 0.51372549) ;
#10985 = CARTESIAN_POINT ( 'NONE',  ( 53.48937290013658696, 122.8810204491430369, 280.0825295754780768 ) ) ;
#10986 =( GEOMETRIC_REPRESENTATION_CONTEXT ( 3 ) GLOBAL_UNCERTAINTY_ASSIGNED_CONTEXT ( ( #10543 ) ) GLOBAL_UNIT_ASSIGNED_CONTEXT ( ( #9171, #16728, #1304 ) ) REPRESENTATION_CONTEXT ( 'NONE', 'WORKASPACE' ) );
#10987 = EDGE_LOOP ( 'NONE', ( #2024, #16377, #11247, #2653 ) ) ;
#10988 = CARTESIAN_POINT ( 'NONE',  ( 53.48937290013658696, 123.1299228374914065, 79.58252780074349175 ) ) ;
#10989 = EDGE_CURVE ( 'NONE', #19951, #17875, #858, .T. ) ;
#10990 = FACE_OUTER_BOUND ( 'NONE', #18382, .T. ) ;
#10991 = DIRECTION ( 'NONE',  ( -0.000000000000000000, -1.000000000000000000, -0.000000000000000000 ) ) ;
#10992 = CARTESIAN_POINT ( 'NONE',  ( 498.8117674897343932, 214.2156642432025251, -87.31255586191144857 ) ) ;
#10993 = PLANE ( 'NONE',  #16569 ) ;
#10994 = CARTESIAN_POINT ( 'NONE',  ( 10.00000000000000000, 372.8685141053778693, -83.18019484660869978 ) ) ;
#10995 = PRESENTATION_STYLE_ASSIGNMENT (( #9235 ) ) ;
#10996 = PRESENTATION_LAYER_ASSIGNMENT (  '', '', ( #9341 ) ) ;
#10997 = ORIENTED_EDGE ( 'NONE', *, *, #7142, .F. ) ;
#10998 = VECTOR ( 'NONE', #18138, 1000.000000000000000 ) ;
#10999 =( GEOMETRIC_REPRESENTATION_CONTEXT ( 3 ) GLOBAL_UNCERTAINTY_ASSIGNED_CONTEXT ( ( #17736 ) ) GLOBAL_UNIT_ASSIGNED_CONTEXT ( ( #637, #19485, #8684 ) ) REPRESENTATION_CONTEXT ( 'NONE', 'WORKASPACE' ) );
#11000 = STYLED_ITEM ( 'NONE', ( #2172 ), #1516 ) ;
#11001 = EDGE_CURVE ( 'NONE', #258, #18079, #3770, .T. ) ;
#11002 = AXIS2_PLACEMENT_3D ( 'NONE', #2552, #15137, #13700 ) ;
#11003 = EDGE_LOOP ( 'NONE', ( #2498, #3053, #3315, #18010 ) ) ;
#11004 = DIRECTION ( 'NONE',  ( 0.000000000000000000, 0.000000000000000000, 1.000000000000000000 ) ) ;
#11005 = CARTESIAN_POINT ( 'NONE',  ( -80.02377347867404467, 140.1169800153989513, 501.4439172727915661 ) ) ;
#11006 = EDGE_LOOP ( 'NONE', ( #5355, #13752 ) ) ;
#11007 = LINE ( 'NONE', #17178, #13652 ) ;
#11008 = EDGE_CURVE ( 'NONE', #17234, #14850, #14580, .T. ) ;
#11009 = ORIENTED_EDGE ( 'NONE', *, *, #10895, .F. ) ;
#11010 = VECTOR ( 'NONE', #16778, 1000.000000000000000 ) ;
#11011 = VECTOR ( 'NONE', #8549, 1000.000000000000000 ) ;
#11012 = MECHANICAL_DESIGN_GEOMETRIC_PRESENTATION_REPRESENTATION (  '', ( #7401 ), #16944 ) ;
#11013 = CARTESIAN_POINT ( 'NONE',  ( 31.00000000000001421, 10.00000000000000000, 25.99999999999999645 ) ) ;
#11014 = DIRECTION ( 'NONE',  ( 0.000000000000000000, 0.000000000000000000, 1.000000000000000000 ) ) ;
#11015 = PRESENTATION_LAYER_ASSIGNMENT (  '', '', ( #20224 ) ) ;
#11016 = DIRECTION ( 'NONE',  ( 0.000000000000000000, 0.000000000000000000, 1.000000000000000000 ) ) ;
#11017 = CARTESIAN_POINT ( 'NONE',  ( 39.99999999999999289, 8.000000000000000000, 26.00000000000000000 ) ) ;
#11018 = DIRECTION ( 'NONE',  ( -1.000000000000000000, 0.000000000000000000, 0.000000000000000000 ) ) ;
#11019 = EDGE_CURVE ( 'NONE', #11867, #14850, #5418, .T. ) ;
#11020 = CARTESIAN_POINT ( 'NONE',  ( 463.8334540492693350, 191.8198460455371333, 158.2339398819845826 ) ) ;
#11021 = VECTOR ( 'NONE', #13521, 1000.000000000000000 ) ;
#11022 = AXIS2_PLACEMENT_3D ( 'NONE', #5334, #11726, #9771 ) ;
#11023 =( NAMED_UNIT ( * ) SI_UNIT ( $, .STERADIAN. ) SOLID_ANGLE_UNIT ( ) );
#11024 = DIRECTION ( 'NONE',  ( 0.000000000000000000, 0.000000000000000000, -1.000000000000000000 ) ) ;
#11025 = EDGE_CURVE ( 'NONE', #2815, #20158, #12489, .T. ) ;
#11026 =( GEOMETRIC_REPRESENTATION_CONTEXT ( 3 ) GLOBAL_UNCERTAINTY_ASSIGNED_CONTEXT ( ( #8588 ) ) GLOBAL_UNIT_ASSIGNED_CONTEXT ( ( #3762, #11896, #2805 ) ) REPRESENTATION_CONTEXT ( 'NONE', 'WORKASPACE' ) );
#11027 = ORIENTED_EDGE ( 'NONE', *, *, #407, .T. ) ;
#11028 = CIRCLE ( 'NONE', #2125, 2.999999999999999112 ) ;
#11029 = AXIS2_PLACEMENT_3D ( 'NONE', #683, #5448, #11737 ) ;
#11030 = ORIENTED_EDGE ( 'NONE', *, *, #1925, .F. ) ;
#11031 = UNCERTAINTY_MEASURE_WITH_UNIT (LENGTH_MEASURE( 1.000000000000000082E-05 ), #4271, 'distance_accuracy_value', 'NONE');
#11032 = VECTOR ( 'NONE', #10192, 1000.000000000000000 ) ;
#11033 = EDGE_CURVE ( 'NONE', #3481, #3254, #5610, .T. ) ;
#11034 = DIRECTION ( 'NONE',  ( 0.000000000000000000, -0.000000000000000000, -1.000000000000000000 ) ) ;
#11035 = ORIENTED_EDGE ( 'NONE', *, *, #8657, .T. ) ;
#11036 = VERTEX_POINT ( 'NONE', #10242 ) ;
#11037 = ORIENTED_EDGE ( 'NONE', *, *, #5484, .T. ) ;
#11038 = CARTESIAN_POINT ( 'NONE',  ( -26.00000000000001776, 10.00000000000000000, 31.00000000000003553 ) ) ;
#11039 = DIRECTION ( 'NONE',  ( 0.000000000000000000, -0.7071067811865336949, -0.7071067811865614505 ) ) ;
#11040 = DIRECTION ( 'NONE',  ( 0.000000000000000000, -0.000000000000000000, 1.000000000000000000 ) ) ;
#11041 = PRESENTATION_LAYER_ASSIGNMENT (  '', '', ( #6427 ) ) ;
#11042 = FACE_OUTER_BOUND ( 'NONE', #16484, .T. ) ;
#11043 = ADVANCED_FACE ( 'NONE', ( #7176 ), #6781, .F. ) ;
#11044 = DIRECTION ( 'NONE',  ( 0.000000000000000000, -0.000000000000000000, 1.000000000000000000 ) ) ;
#11045 = CARTESIAN_POINT ( 'NONE',  ( -81.18192946989263703, 147.7545334744432921, 496.6642397995874489 ) ) ;
#11046 = ADVANCED_FACE ( 'NONE', ( #8498 ), #295, .T. ) ;
#11047 = LINE ( 'NONE', #14037, #16257 ) ;
#11048 = CIRCLE ( 'NONE', #7383, 5.000000000000000888 ) ;
#11049 = VERTEX_POINT ( 'NONE', #11905 ) ;
#11050 = FILL_AREA_STYLE ('',( #6514 ) ) ;
#11051 = FACE_OUTER_BOUND ( 'NONE', #12500, .T. ) ;
#11052 = VECTOR ( 'NONE', #6432, 1000.000000000000000 ) ;
#11053 = B_SPLINE_CURVE_WITH_KNOTS ( 'NONE', 3,
 ( #13889, #3067, #7720, #15677, #12670, #17298, #1509, #18934, #7820, #2862, #4838, #14198, #4527, #6079, #3279, #6483 ),
 .UNSPECIFIED., .F., .F.,
 ( 4, 2, 2, 2, 2, 2, 2, 4 ),
 ( 0.000000000000000000, 0.0005901654530283981324, 0.001180330906056796265, 0.001770496359085194180, 0.002360661812113592530, 0.003540992718170401805, 0.004131158171198806225, 0.004721323624227211080 ),
 .UNSPECIFIED. ) ;
#11054 = CIRCLE ( 'NONE', #12697, 2.000000000000001776 ) ;
#11055 = ORIENTED_EDGE ( 'NONE', *, *, #2522, .T. ) ;
#11056 = DIRECTION ( 'NONE',  ( 1.000000000000000000, 5.889072920838430686E-16, -0.000000000000000000 ) ) ;
#11057 = ORIENTED_EDGE ( 'NONE', *, *, #15439, .F. ) ;
#11058 = ADVANCED_FACE ( 'NONE', ( #11490 ), #19316, .T. ) ;
#11059 = FILL_AREA_STYLE_COLOUR ( '', #1777 ) ;
#11060 = CARTESIAN_POINT ( 'NONE',  ( 78.48937290013660117, 113.1299228374914208, 29.36128450348865471 ) ) ;
#11061 = ORIENTED_EDGE ( 'NONE', *, *, #19901, .F. ) ;
#11062 = FACE_BOUND ( 'NONE', #221, .T. ) ;
#11063 = FACE_OUTER_BOUND ( 'NONE', #10419, .T. ) ;
#11064 = ADVANCED_FACE ( 'NONE', ( #11590 ), #17773, .F. ) ;
#11065 = CARTESIAN_POINT ( 'NONE',  ( 0.4596639520886662278, 140.5461004730986474, 500.9794230863846565 ) ) ;
#11066 = LINE ( 'NONE', #18679, #8168 ) ;
#11067 = DIRECTION ( 'NONE',  ( 0.000000000000000000, 1.000000000000000000, 0.000000000000000000 ) ) ;
#11068 = EDGE_LOOP ( 'NONE', ( #9270, #690, #19372, #5378 ) ) ;
#11069 = PRESENTATION_STYLE_ASSIGNMENT (( #14250 ) ) ;
#11070 = FACE_OUTER_BOUND ( 'NONE', #4196, .T. ) ;
#11071 = APPLICATION_PROTOCOL_DEFINITION ( 'draft international standard', 'automotive_design', 1998, #5268 ) ;
#11072 = ORIENTED_EDGE ( 'NONE', *, *, #12400, .T. ) ;
#11073 = LINE ( 'NONE', #2915, #3021 ) ;
#11074 = ORIENTED_EDGE ( 'NONE', *, *, #1780, .F. ) ;
#11075 = VERTEX_POINT ( 'NONE', #10352 ) ;
#11076 = EDGE_LOOP ( 'NONE', ( #10138, #14543, #16909, #20357 ) ) ;
#11077 =( GEOMETRIC_REPRESENTATION_CONTEXT ( 3 ) GLOBAL_UNCERTAINTY_ASSIGNED_CONTEXT ( ( #3868 ) ) GLOBAL_UNIT_ASSIGNED_CONTEXT ( ( #2343, #16490, #18215 ) ) REPRESENTATION_CONTEXT ( 'NONE', 'WORKASPACE' ) );
#11078 = CARTESIAN_POINT ( 'NONE',  ( 5.687501635565830327, 0.000000000000000000, 0.000000000000000000 ) ) ;
#11079 = EDGE_CURVE ( 'NONE', #5330, #17994, #6020, .T. ) ;
#11080 = ORIENTED_EDGE ( 'NONE', *, *, #8741, .T. ) ;
#11081 = CARTESIAN_POINT ( 'NONE',  ( 78.48937290013660117, 123.1299228374914208, 79.58252780074349175 ) ) ;
#11082 = DIRECTION ( 'NONE',  ( -0.000000000000000000, -1.000000000000000000, 0.000000000000000000 ) ) ;
#11083 = ORIENTED_EDGE ( 'NONE', *, *, #14193, .F. ) ;
#11084 = LINE ( 'NONE', #20253, #13994 ) ;
#11085 = CARTESIAN_POINT ( 'NONE',  ( 3.324999999999999734, -12.97499999999999964, -1.588979221893690953E-15 ) ) ;
#11086 = CARTESIAN_POINT ( 'NONE',  ( 23.00000000000000711, 68.00000000000000000, -31.00000000000002487 ) ) ;
#11087 = CARTESIAN_POINT ( 'NONE',  ( 35.99999999999999289, 6.000000000000000000, 21.99999999999999645 ) ) ;
#11088 = EDGE_CURVE ( 'NONE', #9264, #3611, #20366, .T. ) ;
#11089 = DIRECTION ( 'NONE',  ( 1.000000000000000000, 9.815121534730718631E-17, -0.000000000000000000 ) ) ;
#11090 = EDGE_LOOP ( 'NONE', ( #12456, #1345, #12204, #3424, #4119, #6246, #1505, #16420, #11429, #13404, #6478, #7764, #9834, #18555, #10764, #16192 ) ) ;
#11091 = LINE ( 'NONE', #162, #16509 ) ;
#11092 = CYLINDRICAL_SURFACE ( 'NONE', #2751, 3.300000000000000711 ) ;
#11093 = FACE_BOUND ( 'NONE', #3062, .T. ) ;
#11094 = CARTESIAN_POINT ( 'NONE',  ( -31.00000000000003197, 3.000000000000000000, -30.99999999999999289 ) ) ;
#11095 = CYLINDRICAL_SURFACE ( 'NONE', #16858, 3.300000000000011369 ) ;
#11096 =( NAMED_UNIT ( * ) PLANE_ANGLE_UNIT ( ) SI_UNIT ( $, .RADIAN. ) );
#11097 = ORIENTED_EDGE ( 'NONE', *, *, #19435, .T. ) ;
#11098 = ORIENTED_EDGE ( 'NONE', *, *, #2492, .F. ) ;
#11099 = AXIS2_PLACEMENT_3D ( 'NONE', #8358, #4958, #11230 ) ;
#11100 = EDGE_LOOP ( 'NONE', ( #6517, #11035, #6862, #3834 ) ) ;
#11101 = CARTESIAN_POINT ( 'NONE',  ( 111.4893729001366012, 125.7247684487574588, 252.0000000000000000 ) ) ;
#11102 = CARTESIAN_POINT ( 'NONE',  ( -80.38765499834516959, 139.8541360342012183, 501.0141826477431550 ) ) ;
#11103 = ADVANCED_FACE ( 'NONE', ( #18581 ), #942, .T. ) ;
#11104 = VERTEX_POINT ( 'NONE', #16952 ) ;
#11105 = CARTESIAN_POINT ( 'NONE',  ( 78.48937290013661539, 80.91625508013694912, 0.000000000000000000 ) ) ;
#11106 = LINE ( 'NONE', #15984, #9293 ) ;
#11107 = EDGE_LOOP ( 'NONE', ( #3276, #9580, #17335, #1110 ) ) ;
#11108 = DIRECTION ( 'NONE',  ( 0.000000000000000000, 1.000000000000000000, 0.000000000000000000 ) ) ;
#11109 = PLANE ( 'NONE',  #76 ) ;
#11110 = DIRECTION ( 'NONE',  ( -1.000000000000000000, -0.000000000000000000, -0.000000000000000000 ) ) ;
#11111 = CARTESIAN_POINT ( 'NONE',  ( -31.81980515339462912, 0.000000000000000000, -31.81980515339465043 ) ) ;
#11112 = FACE_BOUND ( 'NONE', #14327, .T. ) ;
#11113 = DIRECTION ( 'NONE',  ( 0.000000000000000000, 0.000000000000000000, -1.000000000000000000 ) ) ;
#11114 = CARTESIAN_POINT ( 'NONE',  ( -23.00000000000002132, 6.000000000000000000, 37.00000000000000711 ) ) ;
#11115 = DIRECTION ( 'NONE',  ( -0.000000000000000000, 1.000000000000000000, -0.000000000000000000 ) ) ;
#11116 = ADVANCED_FACE ( 'NONE', ( #5825 ), #4476, .F. ) ;
#11117 = VECTOR ( 'NONE', #9555, 1000.000000000000000 ) ;
#11118 = PLANE ( 'NONE',  #8928 ) ;
#11119 = DIRECTION ( 'NONE',  ( 1.000000000000000000, -0.000000000000000000, -0.000000000000000000 ) ) ;
#11120 = ORIENTED_EDGE ( 'NONE', *, *, #6161, .F. ) ;
#11121 = ORIENTED_EDGE ( 'NONE', *, *, #680, .F. ) ;
#11122 = EDGE_LOOP ( 'NONE', ( #1389, #6315, #19305, #5959, #9127, #2828 ) ) ;
#11123 = ORIENTED_EDGE ( 'NONE', *, *, #6765, .F. ) ;
#11124 = ORIENTED_EDGE ( 'NONE', *, *, #2921, .F. ) ;
#11125 = DIRECTION ( 'NONE',  ( 0.000000000000000000, 1.000000000000000000, 0.000000000000000000 ) ) ;
#11126 = LINE ( 'NONE', #1930, #8693 ) ;
#11127 = VECTOR ( 'NONE', #16779, 1000.000000000000000 ) ;
#11128 = DIRECTION ( 'NONE',  ( 1.000000000000000000, -0.000000000000000000, -0.000000000000000000 ) ) ;
#11129 = ADVANCED_FACE ( 'NONE', ( #10753 ), #17043, .F. ) ;
#11130 = DIRECTION ( 'NONE',  ( -0.000000000000000000, 1.000000000000000000, -0.000000000000000000 ) ) ;
#11131 = CARTESIAN_POINT ( 'NONE',  ( 31.81980515339464333, 8.000000000000000000, 31.81980515339463622 ) ) ;
#11132 = SURFACE_SIDE_STYLE ('',( #18848 ) ) ;
#11133 = CARTESIAN_POINT ( 'NONE',  ( 423.8334540492694487, 191.8198460455371333, 14.99421986894475012 ) ) ;
#11134 =( NAMED_UNIT ( * ) SI_UNIT ( $, .STERADIAN. ) SOLID_ANGLE_UNIT ( ) );
#11135 = CARTESIAN_POINT ( 'NONE',  ( -31.00000000000005684, 0.000000000000000000, 23.00000000000000355 ) ) ;
#11136 = DIRECTION ( 'NONE',  ( 0.000000000000000000, 0.000000000000000000, 1.000000000000000000 ) ) ;
#11137 = EDGE_CURVE ( 'NONE', #1376, #16358, #12008, .T. ) ;
#11138 = ORIENTED_EDGE ( 'NONE', *, *, #13715, .T. ) ;
#11139 =( LENGTH_UNIT ( ) NAMED_UNIT ( * ) SI_UNIT ( .MILLI., .METRE. ) );
#11140 = CARTESIAN_POINT ( 'NONE',  ( 0.000000000000000000, 309.2289037985890445, -143.5198051533984085 ) ) ;
#11141 = MECHANICAL_DESIGN_GEOMETRIC_PRESENTATION_REPRESENTATION (  '', ( #6900 ), #11480 ) ;
#11142 = EDGE_CURVE ( 'NONE', #9433, #2901, #4184, .T. ) ;
#11143 = ADVANCED_FACE ( 'NONE', ( #2611 ), #8903, .F. ) ;
#11144 = ORIENTED_EDGE ( 'NONE', *, *, #15590, .F. ) ;
#11145 = ADVANCED_FACE ( 'NONE', ( #16847 ), #13841, .T. ) ;
#11146 = DIRECTION ( 'NONE',  ( -0.000000000000000000, -0.000000000000000000, 1.000000000000000000 ) ) ;
#11147 = ORIENTED_EDGE ( 'NONE', *, *, #19202, .T. ) ;
#11148 = DIRECTION ( 'NONE',  ( -0.000000000000000000, -1.000000000000000000, -0.000000000000000000 ) ) ;
#11149 = CARTESIAN_POINT ( 'NONE',  ( -40.00000000000000711, 8.000000000000000000, -19.00000000000000355 ) ) ;
#11150 = ORIENTED_EDGE ( 'NONE', *, *, #3753, .T. ) ;
#11151 = CARTESIAN_POINT ( 'NONE',  ( -31.00000000000006395, 0.000000000000000000, -25.99999999999999645 ) ) ;
#11152 = DIRECTION ( 'NONE',  ( 0.000000000000000000, 0.000000000000000000, -1.000000000000000000 ) ) ;
#11153 = SURFACE_STYLE_USAGE ( .BOTH. , #3008 ) ;
#11154 = CARTESIAN_POINT ( 'NONE',  ( -0.9641265287173192977, 140.4732238075575026, 501.9632754140384918 ) ) ;
#11155 = LINE ( 'NONE', #17344, #15399 ) ;
#11156 = CARTESIAN_POINT ( 'NONE',  ( -80.99999999999995737, 216.7545334744432921, 488.5655098179835818 ) ) ;
#11157 = DIRECTION ( 'NONE',  ( -1.000000000000000000, -1.047380211910524510E-15, -2.094760423821049019E-15 ) ) ;
#11158 = VERTEX_POINT ( 'NONE', #8077 ) ;
#11159 = FILL_AREA_STYLE_COLOUR ( '', #17391 ) ;
#11160 = LINE ( 'NONE', #15052, #16833 ) ;
#11161 = CARTESIAN_POINT ( 'NONE',  ( -40.00000000000000711, 10.00000000000000000, 26.00000000000000000 ) ) ;
#11162 = CONTEXT_DEPENDENT_SHAPE_REPRESENTATION ( #7368, #4992 ) ;
#11163 = VERTEX_POINT ( 'NONE', #231 ) ;
#11164 = CARTESIAN_POINT ( 'NONE',  ( -79.99999999999995737, 216.7545334744432921, 155.1946179577816167 ) ) ;
#11165 = ORIENTED_EDGE ( 'NONE', *, *, #11417, .T. ) ;
#11166 = PRESENTATION_LAYER_ASSIGNMENT (  '', '', ( #20025 ) ) ;
#11167 = ORIENTED_EDGE ( 'NONE', *, *, #6008, .F. ) ;
#11168 = VECTOR ( 'NONE', #19959, 1000.000000000000000 ) ;
#11169 = VECTOR ( 'NONE', #19438, 1000.000000000000000 ) ;
#11170 = CIRCLE ( 'NONE', #6571, 1.000000000000000888 ) ;
#11171 = ORIENTED_EDGE ( 'NONE', *, *, #12382, .F. ) ;
#11172 = EDGE_CURVE ( 'NONE', #7874, #6793, #11066, .T. ) ;
#11173 = LINE ( 'NONE', #14374, #10712 ) ;
#11174 = EDGE_CURVE ( 'NONE', #14748, #8326, #11155, .T. ) ;
#11175 = VERTEX_POINT ( 'NONE', #1865 ) ;
#11176 = LINE ( 'NONE', #9432, #19233 ) ;
#11177 = EDGE_CURVE ( 'NONE', #5312, #3926, #2210, .T. ) ;
#11178 = SURFACE_SIDE_STYLE ('',( #16897 ) ) ;
#11179 =( NAMED_UNIT ( * ) SI_UNIT ( $, .STERADIAN. ) SOLID_ANGLE_UNIT ( ) );
#11180 =( NAMED_UNIT ( * ) SI_UNIT ( $, .STERADIAN. ) SOLID_ANGLE_UNIT ( ) );
#11181 = AXIS2_PLACEMENT_3D ( 'NONE', #19966, #19655, #10714 ) ;
#11182 =( LENGTH_UNIT ( ) NAMED_UNIT ( * ) SI_UNIT ( .MILLI., .METRE. ) );
#11183 = DIRECTION ( 'NONE',  ( 1.000000000000000000, 0.000000000000000000, 0.000000000000000000 ) ) ;
#11184 = VECTOR ( 'NONE', #5599, 1000.000000000000000 ) ;
#11185 = DIRECTION ( 'NONE',  ( 7.719519468096785259E-14, 0.000000000000000000, 1.000000000000000000 ) ) ;
#11186 = ORIENTED_EDGE ( 'NONE', *, *, #15179, .F. ) ;
#11187 = DIRECTION ( 'NONE',  ( 0.000000000000000000, 1.000000000000000000, 0.000000000000000000 ) ) ;
#11188 = CARTESIAN_POINT ( 'NONE',  ( 55.98937290013660828, 143.7407018517681365, 294.8816803532601512 ) ) ;
#11189 =( NAMED_UNIT ( * ) PLANE_ANGLE_UNIT ( ) SI_UNIT ( $, .RADIAN. ) );
#11190 = LINE ( 'NONE', #845, #8706 ) ;
#11191 = CARTESIAN_POINT ( 'NONE',  ( 0.000000000000000000, 0.000000000000000000, 0.000000000000000000 ) ) ;
#11192 = CARTESIAN_POINT ( 'NONE',  ( -26.00000000000002842, 0.000000000000000000, 31.00000000000003908 ) ) ;
#11193 =( LENGTH_UNIT ( ) NAMED_UNIT ( * ) SI_UNIT ( .MILLI., .METRE. ) );
#11194 = ORIENTED_EDGE ( 'NONE', *, *, #5234, .F. ) ;
#11195 = VECTOR ( 'NONE', #3389, 1000.000000000000000 ) ;
#11196 = ADVANCED_FACE ( 'NONE', ( #11255 ), #3326, .T. ) ;
#11197 = VECTOR ( 'NONE', #17645, 1000.000000000000000 ) ;
#11198 = EDGE_LOOP ( 'NONE', ( #1239, #16051, #276, #15671 ) ) ;
#11199 = SURFACE_STYLE_USAGE ( .BOTH. , #18924 ) ;
#11200 = CARTESIAN_POINT ( 'NONE',  ( -81.00000000000065370, 140.4048636633015406, 500.8237260975782874 ) ) ;
#11201 = ORIENTED_EDGE ( 'NONE', *, *, #4099, .T. ) ;
#11202 = ORIENTED_EDGE ( 'NONE', *, *, #8620, .F. ) ;
#11203 = FACE_OUTER_BOUND ( 'NONE', #14392, .T. ) ;
#11204 = PRESENTATION_STYLE_ASSIGNMENT (( #3064 ) ) ;
#11205 = FACE_BOUND ( 'NONE', #1183, .T. ) ;
#11206 = DIRECTION ( 'NONE',  ( 1.000000000000000000, 5.889072920838430686E-16, -0.000000000000000000 ) ) ;
#11207 = CARTESIAN_POINT ( 'NONE',  ( -21.00000000000002842, 3.000000000000000000, -34.99999999999999289 ) ) ;
#11208 = STYLED_ITEM ( 'NONE', ( #1197 ), #17155 ) ;
#11209 = LINE ( 'NONE', #14102, #11195 ) ;
#11210 = CARTESIAN_POINT ( 'NONE',  ( -1.000000000000001110, 152.4824555358011082, 478.3411705753777596 ) ) ;
#11211 = VECTOR ( 'NONE', #14206, 1000.000000000000000 ) ;
#11212 = CARTESIAN_POINT ( 'NONE',  ( 5.425003271131650706, 12.64814671169700055, 0.000000000000000000 ) ) ;
#11213 = CARTESIAN_POINT ( 'NONE',  ( -44.50085094405407915, 175.4489062796178871, 510.3921618609452935 ) ) ;
#11214 = VERTEX_POINT ( 'NONE', #9305 ) ;
#11215 = FILL_AREA_STYLE ('',( #6702 ) ) ;
#11216 = VERTEX_POINT ( 'NONE', #7775 ) ;
#11217 = UNCERTAINTY_MEASURE_WITH_UNIT (LENGTH_MEASURE( 1.000000000000000082E-05 ), #17449, 'distance_accuracy_value', 'NONE');
#11218 = CARTESIAN_POINT ( 'NONE',  ( 423.8334540492694487, 191.8198460455371333, 91.76606011801541740 ) ) ;
#11219 = VERTEX_POINT ( 'NONE', #14453 ) ;
#11220 = MECHANICAL_DESIGN_GEOMETRIC_PRESENTATION_REPRESENTATION (  '', ( #4981 ), #2994 ) ;
#11221 = ORIENTED_EDGE ( 'NONE', *, *, #14062, .F. ) ;
#11222 = CARTESIAN_POINT ( 'NONE',  ( 23.00000000000000711, 0.000000000000000000, -31.00000000000002487 ) ) ;
#11223 = PRESENTATION_LAYER_ASSIGNMENT (  '', '', ( #3992 ) ) ;
#11224 =( NAMED_UNIT ( * ) PLANE_ANGLE_UNIT ( ) SI_UNIT ( $, .RADIAN. ) );
#11225 = DIRECTION ( 'NONE',  ( 0.000000000000000000, 0.000000000000000000, -1.000000000000000000 ) ) ;
#11226 = CARTESIAN_POINT ( 'NONE',  ( -1.170604780609796557E-14, 142.0976792249508946, 502.3210940490797611 ) ) ;
#11227 = LINE ( 'NONE', #16016, #5475 ) ;
#11228 = PRODUCT_DEFINITION_SHAPE ( 'NONE', 'NONE',  #20379 ) ;
#11229 = EDGE_LOOP ( 'NONE', ( #15035, #6821 ) ) ;
#11230 = DIRECTION ( 'NONE',  ( 0.000000000000000000, -0.6235460666509320404, 0.7817866094812263578 ) ) ;
#11231 = DIRECTION ( 'NONE',  ( 0.000000000000000000, 0.000000000000000000, -1.000000000000000000 ) ) ;
#11232 = DIRECTION ( 'NONE',  ( 0.000000000000000000, 0.000000000000000000, -1.000000000000000000 ) ) ;
#11233 = SURFACE_STYLE_FILL_AREA ( #8054 ) ;
#11234 = ORIENTED_EDGE ( 'NONE', *, *, #3613, .T. ) ;
#11235 = LINE ( 'NONE', #108, #18236 ) ;
#11236 = EDGE_CURVE ( 'NONE', #12416, #20017, #6532, .T. ) ;
#11237 = DIRECTION ( 'NONE',  ( 0.000000000000000000, -1.000000000000000000, 0.000000000000000000 ) ) ;
#11238 =( GEOMETRIC_REPRESENTATION_CONTEXT ( 3 ) GLOBAL_UNCERTAINTY_ASSIGNED_CONTEXT ( ( #1725 ) ) GLOBAL_UNIT_ASSIGNED_CONTEXT ( ( #15859, #3171, #12548 ) ) REPRESENTATION_CONTEXT ( 'NONE', 'WORKASPACE' ) );
#11239 = ORIENTED_EDGE ( 'NONE', *, *, #1076, .T. ) ;
#11240 = DIRECTION ( 'NONE',  ( 0.000000000000000000, -1.000000000000000000, 0.000000000000000000 ) ) ;
#11241 = ORIENTED_EDGE ( 'NONE', *, *, #6373, .T. ) ;
#11242 = ADVANCED_FACE ( 'NONE', ( #12724 ), #15812, .F. ) ;
#11243 = DIRECTION ( 'NONE',  ( 0.000000000000000000, 0.000000000000000000, 1.000000000000000000 ) ) ;
#11244 = VERTEX_POINT ( 'NONE', #1650 ) ;
#11245 = CARTESIAN_POINT ( 'NONE',  ( -79.99999999999995737, 216.7545334744432921, 495.1946179577816451 ) ) ;
#11246 = CARTESIAN_POINT ( 'NONE',  ( 10.00000000000000000, 376.0487089519837127, -150.0000000000033538 ) ) ;
#11247 = ORIENTED_EDGE ( 'NONE', *, *, #8692, .T. ) ;
#11248 = CARTESIAN_POINT ( 'NONE',  ( 498.8117674897343932, 214.2156642432025251, -87.31255586191144857 ) ) ;
#11249 =( LENGTH_UNIT ( ) NAMED_UNIT ( * ) SI_UNIT ( .MILLI., .METRE. ) );
#11250 = DIRECTION ( 'NONE',  ( 0.000000000000000000, 1.000000000000000000, 0.000000000000000000 ) ) ;
#11251 = EDGE_CURVE ( 'NONE', #14996, #14515, #15618, .T. ) ;
#11252 = VECTOR ( 'NONE', #5739, 1000.000000000000000 ) ;
#11253 = CARTESIAN_POINT ( 'NONE',  ( -0.3034418303818310347, 139.7372778959907578, 500.7550088380377247 ) ) ;
#11254 = EDGE_CURVE ( 'NONE', #5413, #5205, #15918, .T. ) ;
#11255 = FACE_OUTER_BOUND ( 'NONE', #18378, .T. ) ;
#11256 = FACE_OUTER_BOUND ( 'NONE', #17018, .T. ) ;
#11257 = CARTESIAN_POINT ( 'NONE',  ( -79.04867202909733237, 139.0343723396696873, 488.8251854762526136 ) ) ;
#11258 = AXIS2_PLACEMENT_3D ( 'NONE', #8440, #16184, #19429 ) ;
#11259 = ORIENTED_EDGE ( 'NONE', *, *, #3207, .T. ) ;
#11260 = DIRECTION ( 'NONE',  ( -0.000000000000000000, -1.000000000000000000, -0.000000000000000000 ) ) ;
#11261 = CARTESIAN_POINT ( 'NONE',  ( 31.00000000000000000, 11.00000000000000000, -26.00000000000000355 ) ) ;
#11262 = EDGE_CURVE ( 'NONE', #2973, #10724, #12444, .T. ) ;
#11263 = ORIENTED_EDGE ( 'NONE', *, *, #3599, .T. ) ;
#11264 = COLOUR_RGB ( '', 0.72549020, 0.75294118, 0.79215686) ;
#11265 = ORIENTED_EDGE ( 'NONE', *, *, #15569, .F. ) ;
#11266 = ORIENTED_EDGE ( 'NONE', *, *, #5226, .T. ) ;
#11267 = ORIENTED_EDGE ( 'NONE', *, *, #12799, .F. ) ;
#11268 = FILL_AREA_STYLE_COLOUR ( '', #17628 ) ;
#11269 = EDGE_CURVE ( 'NONE', #19399, #4616, #3559, .T. ) ;
#11270 = DIRECTION ( 'NONE',  ( 0.000000000000000000, 1.000000000000000000, 0.000000000000000000 ) ) ;
#11271 = AXIS2_PLACEMENT_3D ( 'NONE', #18348, #7243, #16158 ) ;
#11272 = VERTEX_POINT ( 'NONE', #14055 ) ;
#11273 = VECTOR ( 'NONE', #17028, 1000.000000000000000 ) ;
#11274 = DIRECTION ( 'NONE',  ( 0.000000000000000000, 1.000000000000000000, 0.000000000000000000 ) ) ;
#11275 = ORIENTED_EDGE ( 'NONE', *, *, #20106, .F. ) ;
#11276 = FILL_AREA_STYLE ('',( #17769 ) ) ;
#11277 = CIRCLE ( 'NONE', #6353, 36.00000000000000000 ) ;
#11278 = CIRCLE ( 'NONE', #12281, 10.00000000000000888 ) ;
#11279 = CARTESIAN_POINT ( 'NONE',  ( -80.47490325750347040, 139.7918628025659586, 489.4274594641468639 ) ) ;
#11280 = EDGE_CURVE ( 'NONE', #548, #6758, #17536, .T. ) ;
#11281 = CARTESIAN_POINT ( 'NONE',  ( -2.844582250340501162, 40.02709031926097083, 9.064464814046603536 ) ) ;
#11282 = ORIENTED_EDGE ( 'NONE', *, *, #3159, .F. ) ;
#11283 =( NAMED_UNIT ( * ) SI_UNIT ( $, .STERADIAN. ) SOLID_ANGLE_UNIT ( ) );
#11284 = FACE_OUTER_BOUND ( 'NONE', #20241, .T. ) ;
#11285 =( LENGTH_UNIT ( ) NAMED_UNIT ( * ) SI_UNIT ( .MILLI., .METRE. ) );
#11286 = LINE ( 'NONE', #9535, #6714 ) ;
#11287 =( LENGTH_UNIT ( ) NAMED_UNIT ( * ) SI_UNIT ( .MILLI., .METRE. ) );
#11288 = EDGE_CURVE ( 'NONE', #19445, #3672, #10792, .T. ) ;
#11289 = ORIENTED_EDGE ( 'NONE', *, *, #9894, .F. ) ;
#11290 = CLOSED_SHELL ( 'NONE', ( #11553, #2924, #8037, #8494, #5371, #16856, #4833, #6282, #5498, #10198, #11064, #2347, #15737, #20070, #15200, #13447, #6121, #19788, #11409, #17650 ) ) ;
#11291 = LINE ( 'NONE', #3673, #3687 ) ;
#11292 = AXIS2_PLACEMENT_3D ( 'NONE', #13792, #12070, #19965 ) ;
#11293 = DIRECTION ( 'NONE',  ( 6.263247009234063646E-17, -0.6381222063396385646, 0.7699350945217602327 ) ) ;
#11294 = ORIENTED_EDGE ( 'NONE', *, *, #17055, .F. ) ;
#11295 = ORIENTED_EDGE ( 'NONE', *, *, #5155, .T. ) ;
#11296 = VECTOR ( 'NONE', #16637, 1000.000000000000000 ) ;
#11297 = CIRCLE ( 'NONE', #16272, 0.9999999999999950040 ) ;
#11298 = ORIENTED_EDGE ( 'NONE', *, *, #2427, .T. ) ;
#11299 = FACE_OUTER_BOUND ( 'NONE', #14353, .T. ) ;
#11300 = ORIENTED_EDGE ( 'NONE', *, *, #667, .T. ) ;
#11301 = DIRECTION ( 'NONE',  ( 1.000000000000000000, 5.889072920838430686E-16, -0.000000000000000000 ) ) ;
#11302 = COLOUR_RGB ( '', 0.72549020, 0.75294118, 0.79215686) ;
#11303 = EDGE_CURVE ( 'NONE', #14242, #17347, #9721, .T. ) ;
#11304 = EDGE_LOOP ( 'NONE', ( #8407, #15912, #15440, #17207 ) ) ;
#11305 = CARTESIAN_POINT ( 'NONE',  ( -79.99999999999995737, 216.7545334744432921, 155.1946179577816167 ) ) ;
#11306 = DIRECTION ( 'NONE',  ( 0.000000000000000000, 1.000000000000000000, 0.000000000000000000 ) ) ;
#11307 = PRESENTATION_STYLE_ASSIGNMENT (( #1825 ) ) ;
#11308 = CARTESIAN_POINT ( 'NONE',  ( -1.242741617435013737E-14, 141.6406393683235194, 501.8237260975781737 ) ) ;
#11309 = EDGE_CURVE ( 'NONE', #17347, #11940, #4570, .T. ) ;
#11310 = DIRECTION ( 'NONE',  ( 0.000000000000000000, -0.000000000000000000, -1.000000000000000000 ) ) ;
#11311 = VECTOR ( 'NONE', #8022, 1000.000000000000000 ) ;
#11312 =( GEOMETRIC_REPRESENTATION_CONTEXT ( 3 ) GLOBAL_UNCERTAINTY_ASSIGNED_CONTEXT ( ( #5795 ) ) GLOBAL_UNIT_ASSIGNED_CONTEXT ( ( #17140, #16043, #1463 ) ) REPRESENTATION_CONTEXT ( 'NONE', 'WORKASPACE' ) );
#11313 = CARTESIAN_POINT ( 'NONE',  ( 53.48937290013658696, 113.1299228374914065, 29.36128450348865471 ) ) ;
#11314 = FILL_AREA_STYLE_COLOUR ( '', #1805 ) ;
#11315 = DIRECTION ( 'NONE',  ( 0.6294249519366466039, -0.7770612780724246438, 9.516256069327462658E-17 ) ) ;
#11316 = PRESENTATION_LAYER_ASSIGNMENT (  '', '', ( #11990 ) ) ;
#11317 = LINE ( 'NONE', #11524, #7226 ) ;
#11318 = CARTESIAN_POINT ( 'NONE',  ( -1.000000000000014655, 152.4824555358010798, 501.3921618609452366 ) ) ;
#11319 = ORIENTED_EDGE ( 'NONE', *, *, #8122, .F. ) ;
#11320 =( GEOMETRIC_REPRESENTATION_CONTEXT ( 3 ) GLOBAL_UNCERTAINTY_ASSIGNED_CONTEXT ( ( #4178 ) ) GLOBAL_UNIT_ASSIGNED_CONTEXT ( ( #19450, #18014, #7015 ) ) REPRESENTATION_CONTEXT ( 'NONE', 'WORKASPACE' ) );
#11321 = VERTEX_POINT ( 'NONE', #6226 ) ;
#11322 = VECTOR ( 'NONE', #6245, 1000.000000000000000 ) ;
#11323 = ORIENTED_EDGE ( 'NONE', *, *, #9885, .T. ) ;
#11324 = SURFACE_STYLE_USAGE ( .BOTH. , #1726 ) ;
#11325 = ORIENTED_EDGE ( 'NONE', *, *, #2166, .T. ) ;
#11326 = ORIENTED_EDGE ( 'NONE', *, *, #6975, .F. ) ;
#11327 = CIRCLE ( 'NONE', #11997, 3.300000000000025135 ) ;
#11328 = AXIS2_PLACEMENT_3D ( 'NONE', #16022, #1948, #4964 ) ;
#11329 = ORIENTED_EDGE ( 'NONE', *, *, #13087, .F. ) ;
#11330 = CARTESIAN_POINT ( 'NONE',  ( 0.9999999999998859801, 216.7545334744432921, 500.8237260975781737 ) ) ;
#11331 = LINE ( 'NONE', #8760, #17570 ) ;
#11332 = AXIS2_PLACEMENT_3D ( 'NONE', #19458, #11549, #706 ) ;
#11333 = CARTESIAN_POINT ( 'NONE',  ( 26.00000000000000355, 11.00000000000000000, -31.00000000000004263 ) ) ;
#11334 = DIRECTION ( 'NONE',  ( 0.000000000000000000, 0.000000000000000000, 1.000000000000000000 ) ) ;
#11335 = FACE_OUTER_BOUND ( 'NONE', #9810, .T. ) ;
#11336 = VECTOR ( 'NONE', #9678, 1000.000000000000000 ) ;
#11337 = FACE_OUTER_BOUND ( 'NONE', #15101, .T. ) ;
#11338 = CARTESIAN_POINT ( 'NONE',  ( 133.4893729001365443, 113.1299228374914634, 170.4174721992565082 ) ) ;
#11339 = VECTOR ( 'NONE', #18722, 1000.000000000000000 ) ;
#11340 = DIRECTION ( 'NONE',  ( 0.000000000000000000, 0.000000000000000000, -1.000000000000000000 ) ) ;
#11341 = DIRECTION ( 'NONE',  ( -1.000000000000000000, 0.000000000000000000, 0.000000000000000000 ) ) ;
#11342 = PLANE ( 'NONE',  #14498 ) ;
#11343 = EDGE_CURVE ( 'NONE', #14259, #15368, #4668, .T. ) ;
#11344 = LINE ( 'NONE', #1433, #3113 ) ;
#11345 = AXIS2_PLACEMENT_3D ( 'NONE', #9112, #1553, #7476 ) ;
#11346 = AXIS2_PLACEMENT_3D ( 'NONE', #17045, #15813, #4477 ) ;
#11347 = LINE ( 'NONE', #17933, #3455 ) ;
#11348 = MECHANICAL_DESIGN_GEOMETRIC_PRESENTATION_REPRESENTATION (  '', ( #2127 ), #3457 ) ;
#11349 = MECHANICAL_DESIGN_GEOMETRIC_PRESENTATION_REPRESENTATION (  '', ( #20224 ), #17759 ) ;
#11350 = EDGE_LOOP ( 'NONE', ( #17387, #18757, #16913, #3809 ) ) ;
#11351 = AXIS2_PLACEMENT_3D ( 'NONE', #15153, #12076, #20020 ) ;
#11352 = FILL_AREA_STYLE_COLOUR ( '', #5778 ) ;
#11353 = ORIENTED_EDGE ( 'NONE', *, *, #13535, .F. ) ;
#11354 = VECTOR ( 'NONE', #5871, 1000.000000000000000 ) ;
#11355 = CARTESIAN_POINT ( 'NONE',  ( 111.4893729001366012, 129.7247684487574588, 370.0000000000000000 ) ) ;
#11356 = ORIENTED_EDGE ( 'NONE', *, *, #6217, .F. ) ;
#11357 = EDGE_CURVE ( 'NONE', #867, #6703, #3132, .T. ) ;
#11358 = CONICAL_SURFACE ( 'NONE', #2474, 13.62500000000000000, 0.2281026282799422378 ) ;
#11359 = FACE_OUTER_BOUND ( 'NONE', #15815, .T. ) ;
#11360 = UNCERTAINTY_MEASURE_WITH_UNIT (LENGTH_MEASURE( 1.000000000000000082E-05 ), #17025, 'distance_accuracy_value', 'NONE');
#11361 = AXIS2_PLACEMENT_3D ( 'NONE', #7805, #18500, #13873 ) ;
#11362 = VERTEX_POINT ( 'NONE', #12927 ) ;
#11363 = LINE ( 'NONE', #4876, #10708 ) ;
#11364 = SURFACE_STYLE_USAGE ( .BOTH. , #9920 ) ;
#11365 = AXIS2_PLACEMENT_3D ( 'NONE', #3035, #7887, #19222 ) ;
#11366 = SURFACE_STYLE_USAGE ( .BOTH. , #327 ) ;
#11367 = SURFACE_SIDE_STYLE ('',( #328 ) ) ;
#11368 = DIRECTION ( 'NONE',  ( 0.000000000000000000, 1.000000000000000000, 0.000000000000000000 ) ) ;
#11369 = MECHANICAL_DESIGN_GEOMETRIC_PRESENTATION_REPRESENTATION (  '', ( #5450 ), #6792 ) ;
#11370 =( NAMED_UNIT ( * ) PLANE_ANGLE_UNIT ( ) SI_UNIT ( $, .RADIAN. ) );
#11371 = CARTESIAN_POINT ( 'NONE',  ( -79.96164301880533287, 139.1521635470821536, 488.4177740748586984 ) ) ;
#11372 = CARTESIAN_POINT ( 'NONE',  ( -0.000000000000000000, 167.9162550801369491, 250.0000000000000000 ) ) ;
#11373 = ORIENTED_EDGE ( 'NONE', *, *, #10239, .T. ) ;
#11374 = SURFACE_STYLE_FILL_AREA ( #6759 ) ;
#11375 = CYLINDRICAL_SURFACE ( 'NONE', #20080, 2.500000000000002220 ) ;
#11376 =( NAMED_UNIT ( * ) PLANE_ANGLE_UNIT ( ) SI_UNIT ( $, .RADIAN. ) );
#11377 = CIRCLE ( 'NONE', #14009, 3.000000000000002665 ) ;
#11378 = EDGE_CURVE ( 'NONE', #1858, #12290, #14552, .T. ) ;
#11379 = EDGE_LOOP ( 'NONE', ( #13296, #10563, #2306, #16835 ) ) ;
#11380 = DIRECTION ( 'NONE',  ( -1.000000000000000000, 2.277380563333649802E-16, 0.000000000000000000 ) ) ;
#11381 = ORIENTED_EDGE ( 'NONE', *, *, #8485, .T. ) ;
#11382 = EDGE_CURVE ( 'NONE', #18513, #7061, #18017, .T. ) ;
#11383 = ORIENTED_EDGE ( 'NONE', *, *, #8862, .F. ) ;
#11384 = EDGE_LOOP ( 'NONE', ( #6475, #10827 ) ) ;
#11385 = AXIS2_PLACEMENT_3D ( 'NONE', #10122, #13335, #11776 ) ;
#11386 = CARTESIAN_POINT ( 'NONE',  ( 78.48937290013660117, 103.1299228374914065, 29.36128450348865471 ) ) ;
#11387 = FILL_AREA_STYLE ('',( #912 ) ) ;
#11388 = ORIENTED_EDGE ( 'NONE', *, *, #10646, .F. ) ;
#11389 = CARTESIAN_POINT ( 'NONE',  ( 493.8117674897343363, 214.2156642432025251, 245.0000000000000000 ) ) ;
#11390 = DIRECTION ( 'NONE',  ( 1.000000000000000000, 0.000000000000000000, 0.000000000000000000 ) ) ;
#11391 = ORIENTED_EDGE ( 'NONE', *, *, #7079, .T. ) ;
#11392 = LINE ( 'NONE', #12843, #7994 ) ;
#11393 = ADVANCED_FACE ( 'NONE', ( #14978 ), #541, .F. ) ;
#11394 =( NAMED_UNIT ( * ) PLANE_ANGLE_UNIT ( ) SI_UNIT ( $, .RADIAN. ) );
#11395 = DIRECTION ( 'NONE',  ( 1.000000000000000000, 5.889072920838430686E-16, -0.000000000000000000 ) ) ;
#11396 = DIRECTION ( 'NONE',  ( 5.889072920838430686E-16, -1.000000000000000000, 0.000000000000000000 ) ) ;
#11397 = PLANE ( 'NONE',  #2762 ) ;
#11398 = VERTEX_POINT ( 'NONE', #3939 ) ;
#11399 = DIRECTION ( 'NONE',  ( -1.000000000000000000, -0.000000000000000000, -0.000000000000000000 ) ) ;
#11400 = FACE_OUTER_BOUND ( 'NONE', #6174, .T. ) ;
#11401 = SURFACE_SIDE_STYLE ('',( #5522 ) ) ;
#11402 = DIRECTION ( 'NONE',  ( -1.047444401652940007E-14, -3.491481338843133355E-15, -1.000000000000000000 ) ) ;
#11403 = VECTOR ( 'NONE', #16711, 1000.000000000000000 ) ;
#11404 = ADVANCED_FACE ( 'NONE', ( #8387 ), #17654, .F. ) ;
#11405 = ORIENTED_EDGE ( 'NONE', *, *, #17077, .F. ) ;
#11406 = DIRECTION ( 'NONE',  ( 0.000000000000000000, -1.000000000000000000, 0.000000000000000000 ) ) ;
#11407 = DIRECTION ( 'NONE',  ( -1.000000000000000000, 0.000000000000000000, 1.322948291343117631E-12 ) ) ;
#11408 = ORIENTED_EDGE ( 'NONE', *, *, #20336, .F. ) ;
#11409 = ADVANCED_FACE ( 'NONE', ( #5495 ), #6946, .F. ) ;
#11410 = ORIENTED_EDGE ( 'NONE', *, *, #19943, .T. ) ;
#11411 = EDGE_CURVE ( 'NONE', #13085, #2774, #19478, .T. ) ;
#11412 = PRODUCT ( 'Part10^Assem2', 'Part10^Assem2', '', ( #18285 ) ) ;
#11413 = ORIENTED_EDGE ( 'NONE', *, *, #14830, .F. ) ;
#11414 = CARTESIAN_POINT ( 'NONE',  ( -1.387778780781445676E-14, 216.7545334744432921, 489.5655098179848892 ) ) ;
#11415 = CARTESIAN_POINT ( 'NONE',  ( 35.99999999999999289, 8.000000000000000000, 18.99999999999999289 ) ) ;
#11416 = ORIENTED_EDGE ( 'NONE', *, *, #12538, .T. ) ;
#11417 = EDGE_CURVE ( 'NONE', #5899, #6147, #5291, .T. ) ;
#11418 = LINE ( 'NONE', #8515, #9369 ) ;
#11419 = LINE ( 'NONE', #2007, #7961 ) ;
#11420 = EDGE_CURVE ( 'NONE', #4616, #2478, #5393, .T. ) ;
#11421 = ORIENTED_EDGE ( 'NONE', *, *, #3084, .T. ) ;
#11422 = AXIS2_PLACEMENT_3D ( 'NONE', #2215, #10162, #16467 ) ;
#11423 = PLANE ( 'NONE',  #1033 ) ;
#11424 = CARTESIAN_POINT ( 'NONE',  ( 53.48937290013659407, 167.9162550801369491, 250.0000000000000000 ) ) ;
#11425 = CARTESIAN_POINT ( 'NONE',  ( -33.99999999999997158, 3.000000000000000000, -22.99999999999999645 ) ) ;
#11426 = FACE_OUTER_BOUND ( 'NONE', #3341, .T. ) ;
#11427 = CYLINDRICAL_SURFACE ( 'NONE', #402, 10.00000000000000888 ) ;
#11428 = FACE_OUTER_BOUND ( 'NONE', #14314, .T. ) ;
#11429 = ORIENTED_EDGE ( 'NONE', *, *, #3838, .T. ) ;
#11430 = LINE ( 'NONE', #10088, #1999 ) ;
#11431 = CARTESIAN_POINT ( 'NONE',  ( 1.050000000000000044, 0.000000000000000000, 0.000000000000000000 ) ) ;
#11432 = ORIENTED_EDGE ( 'NONE', *, *, #5403, .F. ) ;
#11433 = ORIENTED_EDGE ( 'NONE', *, *, #16475, .T. ) ;
#11434 = ORIENTED_EDGE ( 'NONE', *, *, #2884, .T. ) ;
#11435 = VERTEX_POINT ( 'NONE', #8283 ) ;
#11436 = VERTEX_POINT ( 'NONE', #6754 ) ;
#11437 = EDGE_CURVE ( 'NONE', #19090, #7676, #3744, .T. ) ;
#11438 = CARTESIAN_POINT ( 'NONE',  ( 53.48937290013659407, 129.7247684487574588, 283.6050404526570219 ) ) ;
#11439 = CARTESIAN_POINT ( 'NONE',  ( 36.00000000000000000, 0.000000000000000000, 0.000000000000000000 ) ) ;
#11440 = ADVANCED_FACE ( 'NONE', ( #17848 ), #19386, .T. ) ;
#11441 = PLANE ( 'NONE',  #6390 ) ;
#11442 =( NAMED_UNIT ( * ) PLANE_ANGLE_UNIT ( ) SI_UNIT ( $, .RADIAN. ) );
#11443 = EDGE_CURVE ( 'NONE', #14963, #9239, #2889, .T. ) ;
#11444 = DIRECTION ( 'NONE',  ( 1.000000000000000000, -0.000000000000000000, 0.000000000000000000 ) ) ;
#11445 = DIRECTION ( 'NONE',  ( 1.000000000000000000, 0.000000000000000000, 0.000000000000000000 ) ) ;
#11446 = VECTOR ( 'NONE', #8855, 1000.000000000000000 ) ;
#11447 = CYLINDRICAL_SURFACE ( 'NONE', #565, 1.000000000000000888 ) ;
#11448 = DIRECTION ( 'NONE',  ( 0.000000000000000000, 0.000000000000000000, -1.000000000000000000 ) ) ;
#11449 = DIRECTION ( 'NONE',  ( 0.000000000000000000, 0.000000000000000000, -1.000000000000000000 ) ) ;
#11450 = FILL_AREA_STYLE_COLOUR ( '', #13917 ) ;
#11451 = DIRECTION ( 'NONE',  ( 0.000000000000000000, 1.000000000000000000, 0.000000000000000000 ) ) ;
#11452 = LINE ( 'NONE', #17515, #3111 ) ;
#11453 = ORIENTED_EDGE ( 'NONE', *, *, #9289, .F. ) ;
#11454 = VECTOR ( 'NONE', #17299, 1000.000000000000000 ) ;
#11455 = LINE ( 'NONE', #19369, #15320 ) ;
#11456 = ORIENTED_EDGE ( 'NONE', *, *, #9470, .T. ) ;
#11457 = ADVANCED_FACE ( 'NONE', ( #5896 ), #16927, .F. ) ;
#11458 = LINE ( 'NONE', #13127, #10896 ) ;
#11459 = ORIENTED_EDGE ( 'NONE', *, *, #17227, .T. ) ;
#11460 = FACE_OUTER_BOUND ( 'NONE', #2992, .T. ) ;
#11461 = CARTESIAN_POINT ( 'NONE',  ( 0.000000000000000000, 66.00000000000000000, -5.741599279633704455E-16 ) ) ;
#11462 = ORIENTED_EDGE ( 'NONE', *, *, #6169, .F. ) ;
#11463 = CARTESIAN_POINT ( 'NONE',  ( -41.50085094405408626, 193.0431417881923153, 505.3921618609452935 ) ) ;
#11464 = DIRECTION ( 'NONE',  ( -0.000000000000000000, -1.000000000000000000, 0.000000000000000000 ) ) ;
#11465 = DIRECTION ( 'NONE',  ( 1.000000000000000000, 0.000000000000000000, 0.000000000000000000 ) ) ;
#11466 = FILL_AREA_STYLE_COLOUR ( '', #15332 ) ;
#11467 = SURFACE_STYLE_USAGE ( .BOTH. , #3641 ) ;
#11468 = CARTESIAN_POINT ( 'NONE',  ( -8.881784197001250351E-16, -17.85000000000000142, 2.225795557450314789E-15 ) ) ;
#11469 = DIRECTION ( 'NONE',  ( -1.000000000000000000, -0.000000000000000000, 0.000000000000000000 ) ) ;
#11470 = AXIS2_PLACEMENT_3D ( 'NONE', #14176, #8111, #3038 ) ;
#11471 = VERTEX_POINT ( 'NONE', #1121 ) ;
#11472 = DIRECTION ( 'NONE',  ( 0.000000000000000000, 0.000000000000000000, -1.000000000000000000 ) ) ;
#11473 = DIRECTION ( 'NONE',  ( -0.000000000000000000, -1.000000000000000000, -0.000000000000000000 ) ) ;
#11474 = CARTESIAN_POINT ( 'NONE',  ( -81.18192946989242387, 139.7703989349477354, 489.5655098179833544 ) ) ;
#11475 = DIRECTION ( 'NONE',  ( 3.392348130799086764E-14, 0.000000000000000000, -1.000000000000000000 ) ) ;
#11476 = EDGE_LOOP ( 'NONE', ( #834, #11668, #15738, #17035, #15591, #19973, #1840, #3746 ) ) ;
#11477 = ORIENTED_EDGE ( 'NONE', *, *, #11793, .T. ) ;
#11478 = ORIENTED_EDGE ( 'NONE', *, *, #7490, .T. ) ;
#11479 = CARTESIAN_POINT ( 'NONE',  ( 10.00000000000000000, 309.2289037985890445, -146.8198051533984199 ) ) ;
#11480 =( GEOMETRIC_REPRESENTATION_CONTEXT ( 3 ) GLOBAL_UNCERTAINTY_ASSIGNED_CONTEXT ( ( #11583 ) ) GLOBAL_UNIT_ASSIGNED_CONTEXT ( ( #6330, #6538, #6230 ) ) REPRESENTATION_CONTEXT ( 'NONE', 'WORKASPACE' ) );
#11481 = ORIENTED_EDGE ( 'NONE', *, *, #1098, .F. ) ;
#11482 = DIRECTION ( 'NONE',  ( 0.000000000000000000, 1.000000000000000000, 0.000000000000000000 ) ) ;
#11483 = LINE ( 'NONE', #9840, #13180 ) ;
#11484 = VERTEX_POINT ( 'NONE', #10325 ) ;
#11485 = DIRECTION ( 'NONE',  ( -0.000000000000000000, -0.000000000000000000, -1.000000000000000000 ) ) ;
#11486 = EDGE_CURVE ( 'NONE', #17127, #5083, #2794, .T. ) ;
#11487 = CARTESIAN_POINT ( 'NONE',  ( 111.4893729001366012, 125.7247684487574588, 254.0000000000000000 ) ) ;
#11488 = SURFACE_STYLE_USAGE ( .BOTH. , #19221 ) ;
#11489 = FACE_OUTER_BOUND ( 'NONE', #14988, .T. ) ;
#11490 = FACE_OUTER_BOUND ( 'NONE', #8533, .T. ) ;
#11491 = CARTESIAN_POINT ( 'NONE',  ( 53.48937290013659407, 127.7247684487574588, 254.0000000000000000 ) ) ;
#11492 = PRODUCT_RELATED_PRODUCT_CATEGORY ( 'part', '', ( #4824 ) ) ;
#11493 = ORIENTED_EDGE ( 'NONE', *, *, #13636, .T. ) ;
#11494 = CARTESIAN_POINT ( 'NONE',  ( 22.99999999999995737, 0.000000000000000000, -36.99999999999999289 ) ) ;
#11495 = DIRECTION ( 'NONE',  ( 1.141265444721583757E-16, -1.000000000000000000, 0.000000000000000000 ) ) ;
#11496 = SURFACE_STYLE_USAGE ( .BOTH. , #11401 ) ;
#11497 = MECHANICAL_DESIGN_GEOMETRIC_PRESENTATION_REPRESENTATION (  '', ( #2296 ), #18100 ) ;
#11498 = CARTESIAN_POINT ( 'NONE',  ( -26.00000000000000000, 19.00000000000000000, -31.00000000000003908 ) ) ;
#11499 = AXIS2_PLACEMENT_3D ( 'NONE', #7268, #8809, #20116 ) ;
#11500 = DIRECTION ( 'NONE',  ( 0.000000000000000000, 1.000000000000000000, 0.000000000000000000 ) ) ;
#11501 = EDGE_CURVE ( 'NONE', #15750, #19125, #6017, .T. ) ;
#11502 = VERTEX_POINT ( 'NONE', #920 ) ;
#11503 = ORIENTED_EDGE ( 'NONE', *, *, #16964, .T. ) ;
#11504 = ORIENTED_EDGE ( 'NONE', *, *, #15833, .F. ) ;
#11505 =( LENGTH_UNIT ( ) NAMED_UNIT ( * ) SI_UNIT ( .MILLI., .METRE. ) );
#11506 = CARTESIAN_POINT ( 'NONE',  ( 463.8334540492693350, 214.2156642432025251, 250.0000000000000000 ) ) ;
#11507 = ORIENTED_EDGE ( 'NONE', *, *, #17936, .T. ) ;
#11508 = ADVANCED_FACE ( 'NONE', ( #13729 ), #15384, .T. ) ;
#11509 = PRESENTATION_LAYER_ASSIGNMENT (  '', '', ( #15132 ) ) ;
#11510 = CARTESIAN_POINT ( 'NONE',  ( 25.99999999999997868, 0.000000000000000000, 40.00000000000000711 ) ) ;
#11511 = EDGE_CURVE ( 'NONE', #19976, #17153, #12087, .T. ) ;
#11512 = CIRCLE ( 'NONE', #14132, 3.000000000000009770 ) ;
#11513 =( NAMED_UNIT ( * ) SI_UNIT ( $, .STERADIAN. ) SOLID_ANGLE_UNIT ( ) );
#11514 = ORIENTED_EDGE ( 'NONE', *, *, #8091, .T. ) ;
#11515 = LINE ( 'NONE', #17795, #14801 ) ;
#11516 = DIRECTION ( 'NONE',  ( 1.000000000000000000, 9.815121534730718631E-17, -0.000000000000000000 ) ) ;
#11517 = CARTESIAN_POINT ( 'NONE',  ( -0.9517357342956975774, 139.0345459197187097, 488.8243121191512159 ) ) ;
#11518 = LINE ( 'NONE', #9872, #1414 ) ;
#11519 = EDGE_CURVE ( 'NONE', #16481, #17989, #13438, .T. ) ;
#11520 = CARTESIAN_POINT ( 'NONE',  ( -1.000000000000000888, 138.7545334744432637, 509.3921618609452935 ) ) ;
#11521 = CARTESIAN_POINT ( 'NONE',  ( -34.99999999999996447, 8.000000000000000000, 40.00000000000000711 ) ) ;
#11522 = EDGE_CURVE ( 'NONE', #10759, #4977, #9620, .T. ) ;
#11523 = CARTESIAN_POINT ( 'NONE',  ( 463.8334540492693350, 191.8198460455371333, 225.0057801310552463 ) ) ;
#11524 = CARTESIAN_POINT ( 'NONE',  ( -33.00000000000000000, 10.00000000000000000, -22.00000000000000355 ) ) ;
#11525 = ORIENTED_EDGE ( 'NONE', *, *, #4793, .T. ) ;
#11526 = FILL_AREA_STYLE ('',( #14621 ) ) ;
#11527 = ORIENTED_EDGE ( 'NONE', *, *, #3685, .T. ) ;
#11528 = VECTOR ( 'NONE', #6266, 1000.000000000000000 ) ;
#11529 = EDGE_CURVE ( 'NONE', #1021, #13854, #13822, .T. ) ;
#11530 = AXIS2_PLACEMENT_3D ( 'NONE', #8616, #14914, #16870 ) ;
#11531 = CIRCLE ( 'NONE', #6597, 14.27500000000000036 ) ;
#11532 = EDGE_CURVE ( 'NONE', #17418, #18122, #12261, .T. ) ;
#11533 = EDGE_LOOP ( 'NONE', ( #13109, #18897, #13717, #16127 ) ) ;
#11534 = EDGE_LOOP ( 'NONE', ( #13787, #9911, #12810, #10212, #5529, #18785 ) ) ;
#11535 = EDGE_LOOP ( 'NONE', ( #10968, #8303, #5954, #11030 ) ) ;
#11536 = CARTESIAN_POINT ( 'NONE',  ( 10.00000000000000000, 309.2289037985885898, -83.18019484660915452 ) ) ;
#11537 = PRESENTATION_STYLE_ASSIGNMENT (( #5464 ) ) ;
#11538 = ADVANCED_FACE ( 'NONE', ( #10736, #19674 ), #18139, .T. ) ;
#11539 = DIRECTION ( 'NONE',  ( -0.000000000000000000, -1.000000000000000000, -0.000000000000000000 ) ) ;
#11540 = STYLED_ITEM ( 'NONE', ( #9256 ), #16712 ) ;
#11541 = DIRECTION ( 'NONE',  ( 0.000000000000000000, -1.000000000000000000, 0.000000000000000000 ) ) ;
#11542 = STYLED_ITEM ( 'NONE', ( #19956 ), #7238 ) ;
#11543 = AXIS2_PLACEMENT_3D ( 'NONE', #15919, #17434, #6327 ) ;
#11544 = CARTESIAN_POINT ( 'NONE',  ( 2.383085342081995517, 61.83271933867543169, 9.196931476227284463 ) ) ;
#11545 = LINE ( 'NONE', #3915, #16075 ) ;
#11546 = DIRECTION ( 'NONE',  ( 1.000000000000000000, -0.000000000000000000, -0.000000000000000000 ) ) ;
#11547 = FACE_OUTER_BOUND ( 'NONE', #17462, .T. ) ;
#11548 = STYLED_ITEM ( 'NONE', ( #519 ), #11802 ) ;
#11549 = DIRECTION ( 'NONE',  ( 1.000000000000000000, 0.000000000000000000, 0.000000000000000000 ) ) ;
#11550 = EDGE_CURVE ( 'NONE', #18127, #9405, #5686, .T. ) ;
#11551 = CARTESIAN_POINT ( 'NONE',  ( 0.000000000000000000, 216.7545334744432921, 510.3921618609452935 ) ) ;
#11552 = AXIS2_PLACEMENT_3D ( 'NONE', #2818, #7968, #130 ) ;
#11553 = ADVANCED_FACE ( 'NONE', ( #4251 ), #1013, .F. ) ;
#11554 = PRESENTATION_LAYER_ASSIGNMENT (  '', '', ( #27 ) ) ;
#11555 = VERTEX_POINT ( 'NONE', #4550 ) ;
#11556 = DIRECTION ( 'NONE',  ( -0.000000000000000000, -1.000000000000000000, -0.000000000000000000 ) ) ;
#11557 = UNCERTAINTY_MEASURE_WITH_UNIT (LENGTH_MEASURE( 1.000000000000000082E-05 ), #4182, 'distance_accuracy_value', 'NONE');
#11558 = VERTEX_POINT ( 'NONE', #11135 ) ;
#11559 =( NAMED_UNIT ( * ) PLANE_ANGLE_UNIT ( ) SI_UNIT ( $, .RADIAN. ) );
#11560 = ORIENTED_EDGE ( 'NONE', *, *, #18999, .T. ) ;
#11561 = UNCERTAINTY_MEASURE_WITH_UNIT (LENGTH_MEASURE( 1.000000000000000082E-05 ), #6209, 'distance_accuracy_value', 'NONE');
#11562 = CARTESIAN_POINT ( 'NONE',  ( -81.00000000000127898, 138.8810201506716169, 489.5655098179835818 ) ) ;
#11563 = DIRECTION ( 'NONE',  ( 1.000000000000000000, -0.000000000000000000, 0.000000000000000000 ) ) ;
#11564 = ORIENTED_EDGE ( 'NONE', *, *, #3187, .T. ) ;
#11565 = CARTESIAN_POINT ( 'NONE',  ( 0.3499999999999999778, 0.000000000000000000, 0.000000000000000000 ) ) ;
#11566 = CARTESIAN_POINT ( 'NONE',  ( 458.8334540492693350, 191.8198460455371333, 225.0057801310552463 ) ) ;
#11567 = EDGE_CURVE ( 'NONE', #20055, #17762, #212, .T. ) ;
#11568 = CIRCLE ( 'NONE', #13217, 14.59999999999999964 ) ;
#11569 = CARTESIAN_POINT ( 'NONE',  ( 153.4893729001366864, 113.1299228374914634, 29.36128450348865471 ) ) ;
#11570 = DIRECTION ( 'NONE',  ( -1.156482317317875275E-15, 0.000000000000000000, -1.000000000000000000 ) ) ;
#11571 = DIRECTION ( 'NONE',  ( 0.000000000000000000, 0.000000000000000000, -1.000000000000000000 ) ) ;
#11572 = LINE ( 'NONE', #3941, #4449 ) ;
#11573 = ORIENTED_EDGE ( 'NONE', *, *, #15811, .T. ) ;
#11574 = LINE ( 'NONE', #17856, #19860 ) ;
#11575 = CARTESIAN_POINT ( 'NONE',  ( -8.881784197001250351E-16, 0.000000000000000000, 0.000000000000000000 ) ) ;
#11576 = APPLICATION_CONTEXT ( 'automotive_design' ) ;
#11577 = ORIENTED_EDGE ( 'NONE', *, *, #3052, .T. ) ;
#11578 = ORIENTED_EDGE ( 'NONE', *, *, #15897, .T. ) ;
#11579 = AXIS2_PLACEMENT_3D ( 'NONE', #1490, #8004, #14283 ) ;
#11580 = CARTESIAN_POINT ( 'NONE',  ( 21.00000000000000000, 19.00000000000000000, -31.00000000000003908 ) ) ;
#11581 = CIRCLE ( 'NONE', #9939, 8.000000000000007105 ) ;
#11582 = ORIENTED_EDGE ( 'NONE', *, *, #1812, .T. ) ;
#11583 = UNCERTAINTY_MEASURE_WITH_UNIT (LENGTH_MEASURE( 1.000000000000000082E-05 ), #6330, 'distance_accuracy_value', 'NONE');
#11584 = DIRECTION ( 'NONE',  ( 0.000000000000000000, 0.000000000000000000, 1.000000000000000000 ) ) ;
#11585 = DIRECTION ( 'NONE',  ( 1.632406474348796386E-15, -0.7791332379872890623, -0.6268583551835632539 ) ) ;
#11586 = ORIENTED_EDGE ( 'NONE', *, *, #11486, .T. ) ;
#11587 = LINE ( 'NONE', #10238, #16278 ) ;
#11588 = CARTESIAN_POINT ( 'NONE',  ( 503.8334540492693918, 167.8734308960555950, 250.0000000000000000 ) ) ;
#11589 = DIRECTION ( 'NONE',  ( 0.000000000000000000, 1.000000000000000000, -0.000000000000000000 ) ) ;
#11590 = FACE_OUTER_BOUND ( 'NONE', #17571, .T. ) ;
#11591 = FACE_OUTER_BOUND ( 'NONE', #19204, .T. ) ;
#11592 = VERTEX_POINT ( 'NONE', #17510 ) ;
#11593 = SURFACE_STYLE_USAGE ( .BOTH. , #5320 ) ;
#11594 =( LENGTH_UNIT ( ) NAMED_UNIT ( * ) SI_UNIT ( .MILLI., .METRE. ) );
#11595 = SURFACE_STYLE_USAGE ( .BOTH. , #8312 ) ;
#11596 = AXIS2_PLACEMENT_3D ( 'NONE', #10389, #8745, #2745 ) ;
#11597 = PRESENTATION_LAYER_ASSIGNMENT (  '', '', ( #17176 ) ) ;
#11598 = FACE_OUTER_BOUND ( 'NONE', #17053, .T. ) ;
#11599 = EDGE_CURVE ( 'NONE', #17060, #13107, #18756, .T. ) ;
#11600 = ORIENTED_EDGE ( 'NONE', *, *, #1655, .T. ) ;
#11601 = PLANE ( 'NONE',  #9263 ) ;
#11602 = ORIENTED_EDGE ( 'NONE', *, *, #8954, .T. ) ;
#11603 = VECTOR ( 'NONE', #1253, 1000.000000000000000 ) ;
#11604 = VECTOR ( 'NONE', #18962, 1000.000000000000000 ) ;
#11605 = ORIENTED_EDGE ( 'NONE', *, *, #11522, .T. ) ;
#11606 = ORIENTED_EDGE ( 'NONE', *, *, #18946, .T. ) ;
#11607 = FACE_OUTER_BOUND ( 'NONE', #12717, .T. ) ;
#11608 = LINE ( 'NONE', #5438, #15040 ) ;
#11609 = AXIS2_PLACEMENT_3D ( 'NONE', #9397, #4452, #4653 ) ;
#11610 = EDGE_LOOP ( 'NONE', ( #1379, #14162 ) ) ;
#11611 = DIRECTION ( 'NONE',  ( -1.000000000000000000, 0.000000000000000000, 0.000000000000000000 ) ) ;
#11612 = ORIENTED_EDGE ( 'NONE', *, *, #9764, .T. ) ;
#11613 = ADVANCED_FACE ( 'NONE', ( #7842, #6309 ), #15895, .T. ) ;
#11614 = FACE_OUTER_BOUND ( 'NONE', #8392, .T. ) ;
#11615 = DIRECTION ( 'NONE',  ( 1.000000000000000000, 0.000000000000000000, 0.000000000000000000 ) ) ;
#11616 = CARTESIAN_POINT ( 'NONE',  ( 153.4893729001366864, 103.1299228374914492, 170.4174721992565082 ) ) ;
#11617 = DIRECTION ( 'NONE',  ( 0.000000000000000000, 1.000000000000000000, 0.000000000000000000 ) ) ;
#11618 = VECTOR ( 'NONE', #7747, 1000.000000000000000 ) ;
#11619 = DIRECTION ( 'NONE',  ( 0.000000000000000000, -2.352167425053297897E-16, -1.000000000000000000 ) ) ;
#11620 =( LENGTH_UNIT ( ) NAMED_UNIT ( * ) SI_UNIT ( .MILLI., .METRE. ) );
#11621 = DIRECTION ( 'NONE',  ( 0.000000000000000000, 0.000000000000000000, -1.000000000000000000 ) ) ;
#11622 = CARTESIAN_POINT ( 'NONE',  ( 153.4893729001366580, 145.9162550801369491, 0.000000000000000000 ) ) ;
#11623 = EDGE_LOOP ( 'NONE', ( #7785, #20155 ) ) ;
#11624 = DIRECTION ( 'NONE',  ( -0.000000000000000000, -1.000000000000000000, -0.000000000000000000 ) ) ;
#11625 = DIRECTION ( 'NONE',  ( -0.000000000000000000, -1.000000000000000000, -0.000000000000000000 ) ) ;
#11626 = AXIS2_PLACEMENT_3D ( 'NONE', #2465, #13766, #18494 ) ;
#11627 = VERTEX_POINT ( 'NONE', #19050 ) ;
#11628 = AXIS2_PLACEMENT_3D ( 'NONE', #12044, #9036, #4209 ) ;
#11629 = VECTOR ( 'NONE', #4619, 1000.000000000000000 ) ;
#11630 = EDGE_CURVE ( 'NONE', #1465, #10073, #14226, .T. ) ;
#11631 = ORIENTED_EDGE ( 'NONE', *, *, #10003, .T. ) ;
#11632 = ORIENTED_EDGE ( 'NONE', *, *, #12147, .F. ) ;
#11633 = ADVANCED_FACE ( 'NONE', ( #8 ), #6110, .F. ) ;
#11634 = EDGE_LOOP ( 'NONE', ( #5807, #18, #19347, #18271 ) ) ;
#11635 = VECTOR ( 'NONE', #5876, 1000.000000000000000 ) ;
#11636 = VERTEX_POINT ( 'NONE', #4652 ) ;
#11637 = CARTESIAN_POINT ( 'NONE',  ( 486.8117674897343363, 134.2156642432025251, 245.0000000000000000 ) ) ;
#11638 = LINE ( 'NONE', #5465, #3301 ) ;
#11639 = CYLINDRICAL_SURFACE ( 'NONE', #13614, 1.000000000000000888 ) ;
#11640 =( GEOMETRIC_REPRESENTATION_CONTEXT ( 3 ) GLOBAL_UNCERTAINTY_ASSIGNED_CONTEXT ( ( #10119 ) ) GLOBAL_UNIT_ASSIGNED_CONTEXT ( ( #19963, #16501, #5874 ) ) REPRESENTATION_CONTEXT ( 'NONE', 'WORKASPACE' ) );
#11641 = VECTOR ( 'NONE', #14586, 1000.000000000000000 ) ;
#11642 = CARTESIAN_POINT ( 'NONE',  ( 149.0892156028631348, 80.91625508013694912, 250.0000000000000000 ) ) ;
#11643 = EDGE_CURVE ( 'NONE', #20212, #19071, #15596, .T. ) ;
#11644 = CARTESIAN_POINT ( 'NONE',  ( -39.99999999999997868, 3.000000000000000000, 26.00000000000000355 ) ) ;
#11645 = VECTOR ( 'NONE', #18016, 1000.000000000000000 ) ;
#11646 = CARTESIAN_POINT ( 'NONE',  ( 5.945602903476760126, 0.000000000000000000, 0.000000000000000000 ) ) ;
#11647 = SURFACE_SIDE_STYLE ('',( #17504 ) ) ;
#11648 = FACE_OUTER_BOUND ( 'NONE', #19324, .T. ) ;
#11649 = EDGE_CURVE ( 'NONE', #6545, #16028, #10833, .T. ) ;
#11650 = DIRECTION ( 'NONE',  ( -4.956352788505164254E-16, 0.000000000000000000, 1.000000000000000000 ) ) ;
#11651 = STYLED_ITEM ( 'NONE', ( #8898 ), #1321 ) ;
#11652 = STYLED_ITEM ( 'NONE', ( #14375 ), #192 ) ;
#11653 = CARTESIAN_POINT ( 'NONE',  ( 423.8334540492694487, 191.8198460455371333, 178.2339398819846110 ) ) ;
#11654 = DIRECTION ( 'NONE',  ( 0.000000000000000000, 1.000000000000000000, 0.000000000000000000 ) ) ;
#11655 = EDGE_CURVE ( 'NONE', #323, #6446, #3106, .T. ) ;
#11656 = ORIENTED_EDGE ( 'NONE', *, *, #6117, .T. ) ;
#11657 = AXIS2_PLACEMENT_3D ( 'NONE', #12960, #257, #17775 ) ;
#11658 = ORIENTED_EDGE ( 'NONE', *, *, #2351, .F. ) ;
#11659 = VECTOR ( 'NONE', #1018, 1000.000000000000000 ) ;
#11660 = ORIENTED_EDGE ( 'NONE', *, *, #17630, .F. ) ;
#11661 = VERTEX_POINT ( 'NONE', #6416 ) ;
#11662 = EDGE_CURVE ( 'NONE', #3441, #10110, #9396, .T. ) ;
#11663 = ORIENTED_EDGE ( 'NONE', *, *, #15060, .F. ) ;
#11664 = PRESENTATION_LAYER_ASSIGNMENT (  '', '', ( #1439 ) ) ;
#11665 = FILL_AREA_STYLE ('',( #3634 ) ) ;
#11666 = AXIS2_PLACEMENT_3D ( 'NONE', #18320, #16706, #10402 ) ;
#11667 = LINE ( 'NONE', #3841, #12181 ) ;
#11668 = ORIENTED_EDGE ( 'NONE', *, *, #17336, .F. ) ;
#11669 = MECHANICAL_DESIGN_GEOMETRIC_PRESENTATION_REPRESENTATION (  '', ( #15645 ), #4761 ) ;
#11670 = DIRECTION ( 'NONE',  ( 1.000000000000000000, 0.000000000000000000, 0.000000000000000000 ) ) ;
#11671 = CARTESIAN_POINT ( 'NONE',  ( 40.00000000000003553, 3.000000000000000000, -25.99999999999999645 ) ) ;
#11672 = LINE ( 'NONE', #17951, #18844 ) ;
#11673 = VECTOR ( 'NONE', #1891, 1000.000000000000000 ) ;
#11674 = CIRCLE ( 'NONE', #13639, 8.000000000000000000 ) ;
#11675 = VECTOR ( 'NONE', #14642, 1000.000000000000000 ) ;
#11676 = DIRECTION ( 'NONE',  ( 0.000000000000000000, -1.000000000000000000, 0.000000000000000000 ) ) ;
#11677 = DIRECTION ( 'NONE',  ( -1.017652531801993019E-13, 0.000000000000000000, -1.000000000000000000 ) ) ;
#11678 = DIRECTION ( 'NONE',  ( -0.000000000000000000, 1.000000000000000000, -0.000000000000000000 ) ) ;
#11679 = COLOUR_RGB ( '', 0.40784314, 0.44705882, 0.49803922) ;
#11680 = PRESENTATION_STYLE_ASSIGNMENT (( #5497 ) ) ;
#11681 = VERTEX_POINT ( 'NONE', #6210 ) ;
#11682 = CARTESIAN_POINT ( 'NONE',  ( -79.99999999999995737, 152.4824555358010798, 509.3921618609452935 ) ) ;
#11683 = PRESENTATION_STYLE_ASSIGNMENT (( #14984 ) ) ;
#11684 = CARTESIAN_POINT ( 'NONE',  ( -79.99999999999995737, 216.7545334744432921, 495.1946179577816451 ) ) ;
#11685 = CONTEXT_DEPENDENT_SHAPE_REPRESENTATION ( #15800, #16996 ) ;
#11686 = CIRCLE ( 'NONE', #4439, 36.00000000000000000 ) ;
#11687 = COLOUR_RGB ( '', 0.66274510, 0.83137255, 0.94901961) ;
#11688 = VECTOR ( 'NONE', #8833, 1000.000000000000114 ) ;
#11689 = ADVANCED_FACE ( 'NONE', ( #4762 ), #9281, .F. ) ;
#11690 = ORIENTED_EDGE ( 'NONE', *, *, #9768, .T. ) ;
#11691 = PRESENTATION_LAYER_ASSIGNMENT (  '', '', ( #3794 ) ) ;
#11692 = ORIENTED_EDGE ( 'NONE', *, *, #3052, .F. ) ;
#11693 =( GEOMETRIC_REPRESENTATION_CONTEXT ( 3 ) GLOBAL_UNCERTAINTY_ASSIGNED_CONTEXT ( ( #19576 ) ) GLOBAL_UNIT_ASSIGNED_CONTEXT ( ( #3802, #6695, #6904 ) ) REPRESENTATION_CONTEXT ( 'NONE', 'WORKASPACE' ) );
#11694 = PLANE ( 'NONE',  #15345 ) ;
#11695 = VECTOR ( 'NONE', #2197, 1000.000000000000000 ) ;
#11696 = ORIENTED_EDGE ( 'NONE', *, *, #2501, .T. ) ;
#11697 = EDGE_CURVE ( 'NONE', #1451, #13169, #7943, .T. ) ;
#11698 = LINE ( 'NONE', #3954, #10007 ) ;
#11699 = DIRECTION ( 'NONE',  ( 1.000000000000000000, -0.000000000000000000, -0.000000000000000000 ) ) ;
#11700 = EDGE_LOOP ( 'NONE', ( #849, #16673, #1978, #13238, #2676 ) ) ;
#11701 = CARTESIAN_POINT ( 'NONE',  ( 98.48937290013660117, 80.91625508013694912, 0.000000000000000000 ) ) ;
#11702 = LINE ( 'NONE', #8996, #1079 ) ;
#11703 = CIRCLE ( 'NONE', #9705, 5.000000000000004441 ) ;
#11704 = CARTESIAN_POINT ( 'NONE',  ( -35.00000000000000000, 19.00000000000000000, 20.99999999999999289 ) ) ;
#11705 = UNCERTAINTY_MEASURE_WITH_UNIT (LENGTH_MEASURE( 1.000000000000000082E-05 ), #2654, 'distance_accuracy_value', 'NONE');
#11706 = STYLED_ITEM ( 'NONE', ( #14905 ), #8765 ) ;
#11707 = CARTESIAN_POINT ( 'NONE',  ( -33.99999999999997158, -20.00000000000000000, -22.99999999999999645 ) ) ;
#11708 = FILL_AREA_STYLE_COLOUR ( '', #5569 ) ;
#11709 = CARTESIAN_POINT ( 'NONE',  ( 0.000000000000000000, 0.000000000000000000, -12.00000000000000178 ) ) ;
#11710 = ORIENTED_EDGE ( 'NONE', *, *, #16821, .T. ) ;
#11711 = LINE ( 'NONE', #2299, #2480 ) ;
#11712 = CARTESIAN_POINT ( 'NONE',  ( 10.00000000000000000, 1.106257942394396377E-12, -155.0000000000060254 ) ) ;
#11713 = FILL_AREA_STYLE ('',( #3256 ) ) ;
#11714 = DIRECTION ( 'NONE',  ( 1.000000000000000000, 0.000000000000000000, 0.000000000000000000 ) ) ;
#11715 = CARTESIAN_POINT ( 'NONE',  ( -1.577297320522827404E-12, -19.51799192700298846, 176.5415023676507644 ) ) ;
#11716 = SHAPE_REPRESENTATION ( 'Part13^Assem2', ( #2741 ), #2413 ) ;
#11717 = VERTEX_POINT ( 'NONE', #6831 ) ;
#11718 = LINE ( 'NONE', #16267, #6320 ) ;
#11719 = ORIENTED_EDGE ( 'NONE', *, *, #9494, .T. ) ;
#11720 = CIRCLE ( 'NONE', #2809, 10.00000000000000888 ) ;
#11721 = ORIENTED_EDGE ( 'NONE', *, *, #1611, .T. ) ;
#11722 = ORIENTED_EDGE ( 'NONE', *, *, #9948, .T. ) ;
#11723 = ORIENTED_EDGE ( 'NONE', *, *, #16119, .F. ) ;
#11724 = DIRECTION ( 'NONE',  ( 0.000000000000000000, 0.000000000000000000, -1.000000000000000000 ) ) ;
#11725 = VERTEX_POINT ( 'NONE', #14742 ) ;
#11726 = DIRECTION ( 'NONE',  ( 1.000000000000000000, -0.000000000000000000, -0.000000000000000000 ) ) ;
#11727 = ADVANCED_FACE ( 'NONE', ( #16412, #9901 ), #5178, .F. ) ;
#11728 = DIRECTION ( 'NONE',  ( 0.000000000000000000, 0.000000000000000000, -1.000000000000000000 ) ) ;
#11729 = LINE ( 'NONE', #13277, #17107 ) ;
#11730 = PLANE ( 'NONE',  #1349 ) ;
#11731 = MECHANICAL_DESIGN_GEOMETRIC_PRESENTATION_REPRESENTATION (  '', ( #16672 ), #7771 ) ;
#11732 = CARTESIAN_POINT ( 'NONE',  ( 6.299999999999999822, 18.50000000000000000, 0.000000000000000000 ) ) ;
#11733 = LINE ( 'NONE', #15218, #11010 ) ;
#11734 = CARTESIAN_POINT ( 'NONE',  ( 0.000000000000000000, 38.00000000000000711, 0.9999999999999943379 ) ) ;
#11735 = AXIS2_PLACEMENT_3D ( 'NONE', #299, #4852, #6499 ) ;
#11736 =( NAMED_UNIT ( * ) SI_UNIT ( $, .STERADIAN. ) SOLID_ANGLE_UNIT ( ) );
#11737 = DIRECTION ( 'NONE',  ( 0.000000000000000000, 0.000000000000000000, -1.000000000000000000 ) ) ;
#11738 = LINE ( 'NONE', #19343, #2371 ) ;
#11739 = DIRECTION ( 'NONE',  ( -0.000000000000000000, -1.000000000000000000, 0.000000000000000000 ) ) ;
#11740 = EDGE_LOOP ( 'NONE', ( #752, #12165, #11124, #11481 ) ) ;
#11741 =( NAMED_UNIT ( * ) PLANE_ANGLE_UNIT ( ) SI_UNIT ( $, .RADIAN. ) );
#11742 = ORIENTED_EDGE ( 'NONE', *, *, #7710, .F. ) ;
#11743 = ORIENTED_EDGE ( 'NONE', *, *, #10914, .F. ) ;
#11744 = UNCERTAINTY_MEASURE_WITH_UNIT (LENGTH_MEASURE( 1.000000000000000082E-05 ), #16169, 'distance_accuracy_value', 'NONE');
#11745 = EDGE_CURVE ( 'NONE', #6868, #5490, #8546, .T. ) ;
#11746 = VERTEX_POINT ( 'NONE', #6618 ) ;
#11747 = ORIENTED_EDGE ( 'NONE', *, *, #14133, .T. ) ;
#11748 = ORIENTED_EDGE ( 'NONE', *, *, #19325, .F. ) ;
#11749 = CYLINDRICAL_SURFACE ( 'NONE', #3514, 3.883636366625808911 ) ;
#11750 = AXIS2_PLACEMENT_3D ( 'NONE', #11921, #18185, #6983 ) ;
#11751 = FACE_OUTER_BOUND ( 'NONE', #20316, .T. ) ;
#11752 = CARTESIAN_POINT ( 'NONE',  ( 53.48937290013658696, 113.1299228374914065, 79.58252780074349175 ) ) ;
#11753 = FACE_BOUND ( 'NONE', #5323, .T. ) ;
#11754 = CARTESIAN_POINT ( 'NONE',  ( 22.99999999999998224, 10.00000000000000000, -31.99999999999998579 ) ) ;
#11755 = DIRECTION ( 'NONE',  ( -0.7327934916262990317, 0.6804510993672779895, 0.000000000000000000 ) ) ;
#11756 = DIRECTION ( 'NONE',  ( 1.000000000000000000, 1.314570224013242627E-15, 9.702050138162214733E-16 ) ) ;
#11758 = EDGE_CURVE ( 'NONE', #625, #5827, #6929, .T. ) ;
#11757 = PLANE ( 'NONE',  #5445 ) ;
#11759 = PLANE ( 'NONE',  #19328 ) ;
#11760 = CARTESIAN_POINT ( 'NONE',  ( 3.324999999999999734, 0.000000000000000000, 0.000000000000000000 ) ) ;
#11761 = CARTESIAN_POINT ( 'NONE',  ( -26.00000000000002842, 3.000000000000000000, 34.00000000000000711 ) ) ;
#11762 = FILL_AREA_STYLE ('',( #10005 ) ) ;
#11763 = CARTESIAN_POINT ( 'NONE',  ( 78.48937290013660117, 113.1299228374914208, 170.4174721992565082 ) ) ;
#11764 = EDGE_CURVE ( 'NONE', #8530, #16423, #14173, .T. ) ;
#11765 = ORIENTED_EDGE ( 'NONE', *, *, #370, .T. ) ;
#11766 = VERTEX_POINT ( 'NONE', #3827 ) ;
#11767 = SURFACE_SIDE_STYLE ('',( #10513 ) ) ;
#11768 = UNCERTAINTY_MEASURE_WITH_UNIT (LENGTH_MEASURE( 1.000000000000000082E-05 ), #7591, 'distance_accuracy_value', 'NONE');
#11769 = VERTEX_POINT ( 'NONE', #5372 ) ;
#11770 = EDGE_LOOP ( 'NONE', ( #19017, #3119, #6429, #1875 ) ) ;
#11771 = EDGE_CURVE ( 'NONE', #18646, #12714, #16317, .T. ) ;
#11772 = DIRECTION ( 'NONE',  ( -1.000000000000000000, 0.000000000000000000, 0.000000000000000000 ) ) ;
#11773 = UNCERTAINTY_MEASURE_WITH_UNIT (LENGTH_MEASURE( 1.000000000000000082E-05 ), #17007, 'distance_accuracy_value', 'NONE');
#11774 = SURFACE_SIDE_STYLE ('',( #16732 ) ) ;
#11775 = ORIENTED_EDGE ( 'NONE', *, *, #16002, .F. ) ;
#11776 = DIRECTION ( 'NONE',  ( 7.714098457234357737E-14, 6.938893903907222067E-15, 1.000000000000000000 ) ) ;
#11777 = DIRECTION ( 'NONE',  ( -0.000000000000000000, -1.000000000000000000, -0.000000000000000000 ) ) ;
#11779 = EDGE_CURVE ( 'NONE', #18687, #1243, #609, .T. ) ;
#11778 = CARTESIAN_POINT ( 'NONE',  ( 468.8334540492694487, 134.2156642432025251, 245.0000000000000000 ) ) ;
#11780 = CARTESIAN_POINT ( 'NONE',  ( 0.000000000000000000, 1.106257942394396377E-12, -155.0000000000060254 ) ) ;
#11781 = CARTESIAN_POINT ( 'NONE',  ( 82.88953019741013861, 80.91625508013694912, 245.0000000000000000 ) ) ;
#11782 = CARTESIAN_POINT ( 'NONE',  ( -40.00000000000000711, 10.00000000000000000, -18.00000000000000355 ) ) ;
#11783 = DIRECTION ( 'NONE',  ( -1.000000000000000000, -0.000000000000000000, -0.000000000000000000 ) ) ;
#11784 = ADVANCED_FACE ( 'NONE', ( #3917 ), #11342, .F. ) ;
#11785 = VERTEX_POINT ( 'NONE', #16212 ) ;
#11786 = DIRECTION ( 'NONE',  ( -0.000000000000000000, 1.000000000000000000, -0.000000000000000000 ) ) ;
#11787 = DIRECTION ( 'NONE',  ( 1.318389841742372180E-12, 0.000000000000000000, -1.000000000000000000 ) ) ;
#11788 = VECTOR ( 'NONE', #3438, 1000.000000000000000 ) ;
#11789 = CARTESIAN_POINT ( 'NONE',  ( 0.000000000000000000, 167.9162550801369491, -97.94896630388704750 ) ) ;
#11790 = EDGE_CURVE ( 'NONE', #13550, #13965, #17727, .T. ) ;
#11791 = CIRCLE ( 'NONE', #18343, 10.00000000000000888 ) ;
#11792 = ORIENTED_EDGE ( 'NONE', *, *, #7954, .F. ) ;
#11793 = EDGE_CURVE ( 'NONE', #2161, #12975, #7026, .T. ) ;
#11794 = VERTEX_POINT ( 'NONE', #405 ) ;
#11795 = EDGE_LOOP ( 'NONE', ( #17812, #384 ) ) ;
#11796 =( NAMED_UNIT ( * ) SI_UNIT ( $, .STERADIAN. ) SOLID_ANGLE_UNIT ( ) );
#11797 = CARTESIAN_POINT ( 'NONE',  ( -23.00000000000002132, 10.00000000000000000, 32.00000000000000711 ) ) ;
#11798 = VERTEX_POINT ( 'NONE', #13016 ) ;
#11799 = CARTESIAN_POINT ( 'NONE',  ( 21.99999999999998224, 10.00000000000000000, -35.99999999999999289 ) ) ;
#11800 = FILL_AREA_STYLE ('',( #19908 ) ) ;
#11801 = CARTESIAN_POINT ( 'NONE',  ( 0.000000000000000000, 216.7545334744432921, 495.1946179577816451 ) ) ;
#11802 = ADVANCED_FACE ( 'NONE', ( #2156 ), #19164, .F. ) ;
#11803 = COLOUR_RGB ( '', 0.09019608, 0.27058824, 0.51372549) ;
#11804 = LINE ( 'NONE', #14882, #11695 ) ;
#11805 = DIRECTION ( 'NONE',  ( 0.000000000000000000, 1.000000000000000000, 0.000000000000000000 ) ) ;
#11806 = CARTESIAN_POINT ( 'NONE',  ( 468.8334540492694487, 214.2156642432025251, 245.0000000000000000 ) ) ;
#11807 = ORIENTED_EDGE ( 'NONE', *, *, #14260, .T. ) ;
#11808 = LINE ( 'NONE', #17876, #8187 ) ;
#11809 = DIRECTION ( 'NONE',  ( -8.027491443112700323E-16, -0.7071067811865504593, 0.7071067811865445751 ) ) ;
#11810 = VERTEX_POINT ( 'NONE', #5782 ) ;
#11811 = SURFACE_STYLE_FILL_AREA ( #1147 ) ;
#11812 = ADVANCED_FACE ( 'NONE', ( #14952, #4322 ), #15051, .T. ) ;
#11813 = VERTEX_POINT ( 'NONE', #10602 ) ;
#11814 = EDGE_LOOP ( 'NONE', ( #5230, #3786, #11433, #13146 ) ) ;
#11816 = EDGE_CURVE ( 'NONE', #9120, #11362, #4139, .T. ) ;
#11815 = MECHANICAL_DESIGN_GEOMETRIC_PRESENTATION_REPRESENTATION (  '', ( #9165 ), #9837 ) ;
#11817 = ORIENTED_EDGE ( 'NONE', *, *, #710, .F. ) ;
#11818 = EDGE_CURVE ( 'NONE', #18338, #16622, #979, .T. ) ;
#11819 = ORIENTED_EDGE ( 'NONE', *, *, #20138, .T. ) ;
#11820 = VERTEX_POINT ( 'NONE', #16504 ) ;
#11821 = LINE ( 'NONE', #17036, #3009 ) ;
#11822 = CARTESIAN_POINT ( 'NONE',  ( 31.81980515339464333, 11.00000000000000000, -31.81980515339463622 ) ) ;
#11823 = VERTEX_POINT ( 'NONE', #16716 ) ;
#11824 = PRESENTATION_STYLE_ASSIGNMENT (( #18085 ) ) ;
#11825 = PLANE ( 'NONE',  #7642 ) ;
#11826 = PLANE ( 'NONE',  #20129 ) ;
#11827 =( BOUNDED_CURVE ( )  B_SPLINE_CURVE ( 3, ( #13079, #17683, #8112, #9753 ),
 .UNSPECIFIED., .F., .T. ) 
 B_SPLINE_CURVE_WITH_KNOTS ( ( 4, 4 ),
 ( 1.570796326794896558, 3.141592653589793116 ),
 .UNSPECIFIED. ) 
 CURVE ( )  GEOMETRIC_REPRESENTATION_ITEM ( )  RATIONAL_B_SPLINE_CURVE ( ( 1.000000000000000000, 0.8047378541243649375, 0.8047378541243649375, 1.000000000000000000 ) ) 
 REPRESENTATION_ITEM ( '' )  );
#11828 = CIRCLE ( 'NONE', #13480, 1.000000000000015987 ) ;
#11829 = FILL_AREA_STYLE_COLOUR ( '', #2786 ) ;
#11830 = MECHANICAL_DESIGN_GEOMETRIC_PRESENTATION_REPRESENTATION (  '', ( #13784 ), #3261 ) ;
#11831 = DIRECTION ( 'NONE',  ( 0.000000000000000000, 1.000000000000000000, 0.000000000000000000 ) ) ;
#11832 = DIRECTION ( 'NONE',  ( 1.000000000000000000, 5.889072920838430686E-16, -0.000000000000000000 ) ) ;
#11833 = CARTESIAN_POINT ( 'NONE',  ( -34.99999999999998579, -20.00000000000000000, 21.00000000000000355 ) ) ;
#11834 =( LENGTH_UNIT ( ) NAMED_UNIT ( * ) SI_UNIT ( .MILLI., .METRE. ) );
#11835 = DIRECTION ( 'NONE',  ( -1.000000000000000000, 0.000000000000000000, -0.000000000000000000 ) ) ;
#11836 = SURFACE_SIDE_STYLE ('',( #18200 ) ) ;
#11837 = CARTESIAN_POINT ( 'NONE',  ( -78.99999999999995737, 152.4824555358010798, 509.3921618609452935 ) ) ;
#11838 = UNCERTAINTY_MEASURE_WITH_UNIT (LENGTH_MEASURE( 1.000000000000000082E-05 ), #12358, 'distance_accuracy_value', 'NONE');
#11839 = FILL_AREA_STYLE_COLOUR ( '', #1666 ) ;
#11840 = DIRECTION ( 'NONE',  ( 1.000000000000000000, -0.000000000000000000, 0.000000000000000000 ) ) ;
#11841 = EDGE_LOOP ( 'NONE', ( #12028, #12144 ) ) ;
#11842 = EDGE_CURVE ( 'NONE', #9862, #3967, #19967, .T. ) ;
#11843 = ORIENTED_EDGE ( 'NONE', *, *, #6243, .F. ) ;
#11844 = PRESENTATION_LAYER_ASSIGNMENT (  '', '', ( #3936 ) ) ;
#11845 = VERTEX_POINT ( 'NONE', #11961 ) ;
#11846 = CIRCLE ( 'NONE', #16457, 2.999999999999995559 ) ;
#11847 =( GEOMETRIC_REPRESENTATION_CONTEXT ( 3 ) GLOBAL_UNCERTAINTY_ASSIGNED_CONTEXT ( ( #2403 ) ) GLOBAL_UNIT_ASSIGNED_CONTEXT ( ( #3894, #7496, #17069 ) ) REPRESENTATION_CONTEXT ( 'NONE', 'WORKASPACE' ) );
#11848 = ORIENTED_EDGE ( 'NONE', *, *, #1677, .T. ) ;
#11849 = DIRECTION ( 'NONE',  ( 0.000000000000000000, 0.000000000000000000, 1.000000000000000000 ) ) ;
#11850 = DIRECTION ( 'NONE',  ( 0.000000000000000000, 0.000000000000000000, -1.000000000000000000 ) ) ;
#11851 = CARTESIAN_POINT ( 'NONE',  ( 21.00000000000000000, 19.00000000000000000, -35.00000000000000711 ) ) ;
#11852 = DIRECTION ( 'NONE',  ( -0.000000000000000000, -1.000000000000000000, -0.000000000000000000 ) ) ;
#11853 =( NAMED_UNIT ( * ) SI_UNIT ( $, .STERADIAN. ) SOLID_ANGLE_UNIT ( ) );
#11854 = DIRECTION ( 'NONE',  ( 0.000000000000000000, 1.000000000000000000, 0.000000000000000000 ) ) ;
#11855 = CARTESIAN_POINT ( 'NONE',  ( 111.4893729001366012, 126.1646452518344859, 280.0825295754780768 ) ) ;
#11856 = LINE ( 'NONE', #7219, #4202 ) ;
#11857 = STYLED_ITEM ( 'NONE', ( #10995 ), #16397 ) ;
#11858 = DIRECTION ( 'NONE',  ( -0.000000000000000000, -1.000000000000000000, -0.000000000000000000 ) ) ;
#11859 = LINE ( 'NONE', #18116, #14161 ) ;
#11860 = AXIS2_PLACEMENT_3D ( 'NONE', #2009, #5037, #12875 ) ;
#11861 =( NAMED_UNIT ( * ) PLANE_ANGLE_UNIT ( ) SI_UNIT ( $, .RADIAN. ) );
#11862 = AXIS2_PLACEMENT_3D ( 'NONE', #1027, #13738, #2806 ) ;
#11863 = DIRECTION ( 'NONE',  ( 1.000000000000000000, -0.000000000000000000, 0.000000000000000000 ) ) ;
#11864 = DIRECTION ( 'NONE',  ( 0.000000000000000000, 0.000000000000000000, -1.000000000000000000 ) ) ;
#11865 = EDGE_CURVE ( 'NONE', #1350, #2696, #10413, .T. ) ;
#11866 = ORIENTED_EDGE ( 'NONE', *, *, #12152, .T. ) ;
#11867 = VERTEX_POINT ( 'NONE', #5562 ) ;
#11868 =( NAMED_UNIT ( * ) PLANE_ANGLE_UNIT ( ) SI_UNIT ( $, .RADIAN. ) );
#11869 = ORIENTED_EDGE ( 'NONE', *, *, #2185, .T. ) ;
#11870 = ORIENTED_EDGE ( 'NONE', *, *, #9373, .T. ) ;
#11871 = VECTOR ( 'NONE', #5584, 1000.000000000000000 ) ;
#11872 = CARTESIAN_POINT ( 'NONE',  ( 149.0892156028631348, 167.9162550801369491, 250.0000000000000000 ) ) ;
#11873 = AXIS2_PLACEMENT_3D ( 'NONE', #16822, #1005, #4246 ) ;
#11874 = CARTESIAN_POINT ( 'NONE',  ( 98.48937290013662960, 123.1299228374914350, 220.6387154965113382 ) ) ;
#11875 = FACE_OUTER_BOUND ( 'NONE', #16296, .T. ) ;
#11876 = PRESENTATION_STYLE_ASSIGNMENT (( #10215 ) ) ;
#11877 = DIRECTION ( 'NONE',  ( 1.000000000000000000, 0.000000000000000000, 0.000000000000000000 ) ) ;
#11878 = DIRECTION ( 'NONE',  ( -1.000000000000000000, -0.000000000000000000, -0.000000000000000000 ) ) ;
#11879 = ADVANCED_FACE ( 'NONE', ( #9071 ), #7434, .F. ) ;
#11880 = CYLINDRICAL_SURFACE ( 'NONE', #12703, 9.000000000000007105 ) ;
#11881 = CARTESIAN_POINT ( 'NONE',  ( 153.4893729001366864, 113.1299228374914634, 220.6387154965113382 ) ) ;
#11882 = LINE ( 'NONE', #12175, #11871 ) ;
#11883 = CARTESIAN_POINT ( 'NONE',  ( 468.8334540492694487, 214.2156642432025251, 245.0000000000000000 ) ) ;
#11884 = ORIENTED_EDGE ( 'NONE', *, *, #4238, .T. ) ;
#11885 = SURFACE_SIDE_STYLE ('',( #1126 ) ) ;
#11886 = DIRECTION ( 'NONE',  ( -0.000000000000000000, 1.000000000000000000, -0.000000000000000000 ) ) ;
#11887 = DIRECTION ( 'NONE',  ( -0.000000000000000000, -1.000000000000000000, -0.000000000000000000 ) ) ;
#11888 = AXIS2_PLACEMENT_3D ( 'NONE', #4673, #9511, #15728 ) ;
#11889 = CIRCLE ( 'NONE', #5627, 15.14120580695350071 ) ;
#11890 = PRESENTATION_STYLE_ASSIGNMENT (( #1007 ) ) ;
#11891 = EDGE_CURVE ( 'NONE', #14767, #20158, #20065, .T. ) ;
#11892 = ORIENTED_EDGE ( 'NONE', *, *, #8661, .F. ) ;
#11893 = EDGE_CURVE ( 'NONE', #7970, #7830, #12153, .T. ) ;
#11894 = VERTEX_POINT ( 'NONE', #7132 ) ;
#11895 = VECTOR ( 'NONE', #2867, 1000.000000000000000 ) ;
#11896 =( NAMED_UNIT ( * ) PLANE_ANGLE_UNIT ( ) SI_UNIT ( $, .RADIAN. ) );
#11897 = CARTESIAN_POINT ( 'NONE',  ( 31.00000000000002842, 0.000000000000000000, 26.00000000000001066 ) ) ;
#11898 = ORIENTED_EDGE ( 'NONE', *, *, #6278, .T. ) ;
#11899 = CARTESIAN_POINT ( 'NONE',  ( 21.00000000000000000, 8.000000000000000000, 35.00000000000001421 ) ) ;
#11900 = SURFACE_STYLE_USAGE ( .BOTH. , #938 ) ;
#11901 = FACE_OUTER_BOUND ( 'NONE', #18210, .T. ) ;
#11902 = DIRECTION ( 'NONE',  ( -0.4740998230350218501, -0.8804710999221728729, -1.078266114261438272E-16 ) ) ;
#11903 = EDGE_CURVE ( 'NONE', #3197, #10186, #17793, .T. ) ;
#11904 = CARTESIAN_POINT ( 'NONE',  ( -80.26761590469169505, 140.6967024680590441, 501.1310021303755207 ) ) ;
#11905 = CARTESIAN_POINT ( 'NONE',  ( -23.00000000000002842, 0.000000000000000000, -31.00000000000003553 ) ) ;
#11906 = LINE ( 'NONE', #18163, #19254 ) ;
#11907 = EDGE_LOOP ( 'NONE', ( #19515, #15782, #2778, #9421 ) ) ;
#11908 = EDGE_CURVE ( 'NONE', #20073, #6580, #8770, .T. ) ;
#11909 = DIRECTION ( 'NONE',  ( 1.000000000000000000, 0.000000000000000000, 0.000000000000000000 ) ) ;
#11910 = DIRECTION ( 'NONE',  ( 0.000000000000000000, -0.000000000000000000, -1.000000000000000000 ) ) ;
#11911 = DIRECTION ( 'NONE',  ( 0.000000000000000000, 0.000000000000000000, 1.000000000000000000 ) ) ;
#11912 = VERTEX_POINT ( 'NONE', #13507 ) ;
#11913 = FACE_OUTER_BOUND ( 'NONE', #7529, .T. ) ;
#11914 = ORIENTED_EDGE ( 'NONE', *, *, #4561, .T. ) ;
#11915 = AXIS2_PLACEMENT_3D ( 'NONE', #13876, #969, #18310 ) ;
#11916 = ORIENTED_EDGE ( 'NONE', *, *, #10989, .F. ) ;
#11917 = ADVANCED_FACE ( 'NONE', ( #7315, #12071, #12854, #461, #11284 ), #17009, .F. ) ;
#11918 = EDGE_LOOP ( 'NONE', ( #14249, #362, #474, #599 ) ) ;
#11919 = CYLINDRICAL_SURFACE ( 'NONE', #12365, 5.000000000000000888 ) ;
#11920 = ORIENTED_EDGE ( 'NONE', *, *, #1537, .F. ) ;
#11921 = CARTESIAN_POINT ( 'NONE',  ( 35.00000000000003553, 3.000000000000000000, -20.99999999999999645 ) ) ;
#11922 = ORIENTED_EDGE ( 'NONE', *, *, #8773, .F. ) ;
#11923 = EDGE_CURVE ( 'NONE', #8866, #14088, #19112, .T. ) ;
#11924 = CARTESIAN_POINT ( 'NONE',  ( -39.99999999999997868, 0.000000000000000000, 26.00000000000000355 ) ) ;
#11925 = LINE ( 'NONE', #4096, #8887 ) ;
#11926 = AXIS2_PLACEMENT_3D ( 'NONE', #1046, #18478, #2824 ) ;
#11927 = ADVANCED_FACE ( 'NONE', ( #11400 ), #7616, .F. ) ;
#11928 = DIRECTION ( 'NONE',  ( 0.000000000000000000, 0.000000000000000000, 1.000000000000000000 ) ) ;
#11929 = CARTESIAN_POINT ( 'NONE',  ( 0.000000000000000000, 8.000000000000000000, 0.000000000000000000 ) ) ;
#11930 = FACE_OUTER_BOUND ( 'NONE', #1905, .T. ) ;
#11931 =( NAMED_UNIT ( * ) PLANE_ANGLE_UNIT ( ) SI_UNIT ( $, .RADIAN. ) );
#11932 = FILL_AREA_STYLE ('',( #10274 ) ) ;
#11933 = FILL_AREA_STYLE ('',( #2542 ) ) ;
#11934 = VECTOR ( 'NONE', #10167, 1000.000000000000000 ) ;
#11935 = PRESENTATION_STYLE_ASSIGNMENT (( #5645 ) ) ;
#11936 = PLANE ( 'NONE',  #1939 ) ;
#11937 = ORIENTED_EDGE ( 'NONE', *, *, #12395, .F. ) ;
#11938 = AXIS2_PLACEMENT_3D ( 'NONE', #8502, #660, #3669 ) ;
#11939 = LINE ( 'NONE', #18208, #20227 ) ;
#11940 = VERTEX_POINT ( 'NONE', #8209 ) ;
#11941 = AXIS2_PLACEMENT_3D ( 'NONE', #16830, #7458, #14012 ) ;
#11942 = STYLED_ITEM ( 'NONE', ( #1994 ), #18267 ) ;
#11943 = UNCERTAINTY_MEASURE_WITH_UNIT (LENGTH_MEASURE( 1.000000000000000082E-05 ), #6996, 'distance_accuracy_value', 'NONE');
#11944 = VERTEX_POINT ( 'NONE', #13895 ) ;
#11945 = VECTOR ( 'NONE', #16360, 1000.000000000000000 ) ;
#11947 = ORIENTED_EDGE ( 'NONE', *, *, #11382, .T. ) ;
#11946 = EDGE_CURVE ( 'NONE', #889, #6644, #11827, .T. ) ;
#11948 = DIRECTION ( 'NONE',  ( -0.000000000000000000, -1.000000000000000000, 0.000000000000000000 ) ) ;
#11949 = PLANE ( 'NONE',  #653 ) ;
#11950 = SURFACE_STYLE_USAGE ( .BOTH. , #16605 ) ;
#11951 = MECHANICAL_DESIGN_GEOMETRIC_PRESENTATION_REPRESENTATION (  '', ( #14232 ), #18836 ) ;
#11952 = AXIS2_PLACEMENT_3D ( 'NONE', #10530, #7341, #18661 ) ;
#11953 = EDGE_CURVE ( 'NONE', #19875, #17263, #14484, .T. ) ;
#11954 = CARTESIAN_POINT ( 'NONE',  ( 3.500000000000000000, 14.59999999999999964, 0.000000000000000000 ) ) ;
#11955 = FACE_OUTER_BOUND ( 'NONE', #5626, .T. ) ;
#11956 = CARTESIAN_POINT ( 'NONE',  ( 0.000000000000000000, 34.32473510485366575, 0.000000000000000000 ) ) ;
#11957 = VECTOR ( 'NONE', #2064, 1000.000000000000000 ) ;
#11958 = CIRCLE ( 'NONE', #7038, 3.000000000000002665 ) ;
#11959 = DIRECTION ( 'NONE',  ( -1.000000000000000000, 0.000000000000000000, -0.000000000000000000 ) ) ;
#11960 = CARTESIAN_POINT ( 'NONE',  ( 423.8334540492694487, 191.8198460455371333, 158.2339398819845826 ) ) ;
#11961 = CARTESIAN_POINT ( 'NONE',  ( 36.00000000000000000, 0.000000000000000000, -135.0000000000000284 ) ) ;
#11962 = SURFACE_STYLE_USAGE ( .BOTH. , #13509 ) ;
#11963 = PRESENTATION_STYLE_ASSIGNMENT (( #19659 ) ) ;
#11964 = AXIS2_PLACEMENT_3D ( 'NONE', #6388, #12776, #7822 ) ;
#11965 = VERTEX_POINT ( 'NONE', #5015 ) ;
#11966 = CARTESIAN_POINT ( 'NONE',  ( -31.00000000000002132, 0.000000000000000000, -31.00000000000000000 ) ) ;
#11967 = VERTEX_POINT ( 'NONE', #3572 ) ;
#11968 = ORIENTED_EDGE ( 'NONE', *, *, #805, .F. ) ;
#11969 = MECHANICAL_DESIGN_GEOMETRIC_PRESENTATION_REPRESENTATION (  '', ( #4065 ), #747 ) ;
#11970 = COLOUR_RGB ( '', 0.31764706, 0.68627451, 0.89019608) ;
#11971 = AXIS2_PLACEMENT_3D ( 'NONE', #19957, #983, #15355 ) ;
#11972 = CARTESIAN_POINT ( 'NONE',  ( -80.99999999999995737, 140.4048636633015406, 499.8237260975782874 ) ) ;
#11973 = UNCERTAINTY_MEASURE_WITH_UNIT (LENGTH_MEASURE( 1.000000000000000082E-05 ), #12051, 'distance_accuracy_value', 'NONE');
#11974 = DIRECTION ( 'NONE',  ( -0.000000000000000000, -1.000000000000000000, -0.000000000000000000 ) ) ;
#11975 = APPLICATION_CONTEXT ( 'automotive_design' ) ;
#11976 = CARTESIAN_POINT ( 'NONE',  ( 111.4893729001366012, 119.5973956464515879, 322.0399576098686225 ) ) ;
#11977 = CARTESIAN_POINT ( 'NONE',  ( 109.4893729001366012, 127.7247684487574588, 370.0000000000000000 ) ) ;
#11978 = CARTESIAN_POINT ( 'NONE',  ( -31.00000000000006750, 3.000000000000000000, 26.00000000000000355 ) ) ;
#11979 = AXIS2_PLACEMENT_3D ( 'NONE', #6553, #3249, #18699 ) ;
#11980 = EDGE_CURVE ( 'NONE', #7373, #20355, #10715, .T. ) ;
#11981 = CARTESIAN_POINT ( 'NONE',  ( -31.81980515339462912, 11.00000000000000000, 31.81980515339465043 ) ) ;
#11982 = CARTESIAN_POINT ( 'NONE',  ( -35.00000000000000000, 19.00000000000000000, -21.00000000000000000 ) ) ;
#11983 =( LENGTH_UNIT ( ) NAMED_UNIT ( * ) SI_UNIT ( .MILLI., .METRE. ) );
#11984 = DIRECTION ( 'NONE',  ( -0.000000000000000000, -1.000000000000000000, -0.000000000000000000 ) ) ;
#11985 = ORIENTED_EDGE ( 'NONE', *, *, #15665, .F. ) ;
#11986 = FILL_AREA_STYLE ('',( #2499 ) ) ;
#11987 = SURFACE_SIDE_STYLE ('',( #5901 ) ) ;
#11988 = CARTESIAN_POINT ( 'NONE',  ( 153.4893729001366580, 0.000000000000000000, 0.000000000000000000 ) ) ;
#11989 = MECHANICAL_DESIGN_GEOMETRIC_PRESENTATION_REPRESENTATION (  '', ( #5412 ), #9017 ) ;
#11990 = STYLED_ITEM ( 'NONE', ( #11683 ), #15608 ) ;
#11991 = ORIENTED_EDGE ( 'NONE', *, *, #19640, .F. ) ;
#11992 = CIRCLE ( 'NONE', #5421, 7.999999999999996447 ) ;
#11993 = ORIENTED_EDGE ( 'NONE', *, *, #2695, .F. ) ;
#11994 = EDGE_CURVE ( 'NONE', #5835, #16530, #12368, .T. ) ;
#11995 = UNCERTAINTY_MEASURE_WITH_UNIT (LENGTH_MEASURE( 1.000000000000000082E-05 ), #6608, 'distance_accuracy_value', 'NONE');
#11996 = ORIENTED_EDGE ( 'NONE', *, *, #12673, .F. ) ;
#11997 = AXIS2_PLACEMENT_3D ( 'NONE', #8108, #14695, #6874 ) ;
#11998 = CARTESIAN_POINT ( 'NONE',  ( -30.99999999999999645, 68.00000000000000000, -30.99999999999999289 ) ) ;
#11999 = CARTESIAN_POINT ( 'NONE',  ( -37.00000000000000000, 68.00000000000000000, 23.00000000000000355 ) ) ;
#12000 = UNCERTAINTY_MEASURE_WITH_UNIT (LENGTH_MEASURE( 1.000000000000000082E-05 ), #8048, 'distance_accuracy_value', 'NONE');
#12001 = PRESENTATION_LAYER_ASSIGNMENT (  '', '', ( #7401 ) ) ;
#12002 = ORIENTED_EDGE ( 'NONE', *, *, #19579, .T. ) ;
#12003 = CARTESIAN_POINT ( 'NONE',  ( 0.000000000000000000, 372.8685141053778693, -86.48019484660871115 ) ) ;
#12004 = DIRECTION ( 'NONE',  ( 1.000000000000000000, 0.000000000000000000, 0.000000000000000000 ) ) ;
#12005 = VECTOR ( 'NONE', #16319, 1000.000000000000000 ) ;
#12006 = DIRECTION ( 'NONE',  ( 1.000000000000000000, 5.889072920838430686E-16, -0.000000000000000000 ) ) ;
#12007 = DIRECTION ( 'NONE',  ( 0.000000000000000000, 0.000000000000000000, 1.000000000000000000 ) ) ;
#12008 = LINE ( 'NONE', #6134, #18677 ) ;
#12009 = AXIS2_PLACEMENT_3D ( 'NONE', #17017, #9079, #11034 ) ;
#12010 = EDGE_CURVE ( 'NONE', #13941, #2260, #3322, .T. ) ;
#12011 = DIRECTION ( 'NONE',  ( 0.000000000000000000, 0.000000000000000000, -1.000000000000000000 ) ) ;
#12012 = VECTOR ( 'NONE', #675, 1000.000000000000000 ) ;
#12013 = ORIENTED_EDGE ( 'NONE', *, *, #16115, .F. ) ;
#12014 = DIRECTION ( 'NONE',  ( 0.000000000000000000, 0.000000000000000000, 1.000000000000000000 ) ) ;
#12015 = DIRECTION ( 'NONE',  ( 1.000000000000000000, -0.000000000000000000, 0.000000000000000000 ) ) ;
#12016 = FACE_OUTER_BOUND ( 'NONE', #17529, .T. ) ;
#12017 = APPLICATION_PROTOCOL_DEFINITION ( 'draft international standard', 'automotive_design', 1998, #2871 ) ;
#12018 = AXIS2_PLACEMENT_3D ( 'NONE', #2507, #17039, #7257 ) ;
#12019 = VERTEX_POINT ( 'NONE', #260 ) ;
#12020 = ORIENTED_EDGE ( 'NONE', *, *, #17679, .F. ) ;
#12021 = EDGE_CURVE ( 'NONE', #469, #17405, #14584, .T. ) ;
#12022 = CYLINDRICAL_SURFACE ( 'NONE', #2360, 10.00000000000000888 ) ;
#12023 = PRESENTATION_LAYER_ASSIGNMENT (  '', '', ( #14320 ) ) ;
#12024 = ORIENTED_EDGE ( 'NONE', *, *, #15113, .T. ) ;
#12025 = CIRCLE ( 'NONE', #17934, 10.00000000000000888 ) ;
#12026 = ORIENTED_EDGE ( 'NONE', *, *, #6997, .F. ) ;
#12027 = VECTOR ( 'NONE', #17677, 1000.000000000000000 ) ;
#12028 = ORIENTED_EDGE ( 'NONE', *, *, #3518, .F. ) ;
#12029 = CIRCLE ( 'NONE', #10366, 10.00000000000000888 ) ;
#12030 = DIRECTION ( 'NONE',  ( 0.000000000000000000, 0.000000000000000000, -1.000000000000000000 ) ) ;
#12031 = AXIS2_PLACEMENT_3D ( 'NONE', #8203, #3465, #1885 ) ;
#12032 = ORIENTED_EDGE ( 'NONE', *, *, #6161, .T. ) ;
#12033 = EDGE_CURVE ( 'NONE', #5083, #8090, #11091, .T. ) ;
#12034 = DIRECTION ( 'NONE',  ( 1.000000000000000000, 0.000000000000000000, 0.000000000000000000 ) ) ;
#12035 = STYLED_ITEM ( 'NONE', ( #3592 ), #10774 ) ;
#12036 = ORIENTED_EDGE ( 'NONE', *, *, #9186, .T. ) ;
#12037 = FACE_OUTER_BOUND ( 'NONE', #8065, .T. ) ;
#12038 = DIRECTION ( 'NONE',  ( 1.000000000000000000, 0.000000000000000000, -0.000000000000000000 ) ) ;
#12039 = FILL_AREA_STYLE_COLOUR ( '', #5671 ) ;
#12040 = ADVANCED_FACE ( 'NONE', ( #14277 ), #17372, .F. ) ;
#12041 =( NAMED_UNIT ( * ) SI_UNIT ( $, .STERADIAN. ) SOLID_ANGLE_UNIT ( ) );
#12042 = LINE ( 'NONE', #5849, #14746 ) ;
#12043 = LINE ( 'NONE', #13484, #2372 ) ;
#12044 = CARTESIAN_POINT ( 'NONE',  ( 10.00000000000000000, 1.106257942394396377E-12, -155.0000000000060254 ) ) ;
#12045 = DIRECTION ( 'NONE',  ( 0.000000000000000000, 0.000000000000000000, 1.000000000000000000 ) ) ;
#12046 = PLANE ( 'NONE',  #2457 ) ;
#12047 = SURFACE_STYLE_USAGE ( .BOTH. , #11836 ) ;
#12048 = AXIS2_PLACEMENT_3D ( 'NONE', #325, #6634, #12922 ) ;
#12049 = LINE ( 'NONE', #7404, #15466 ) ;
#12050 = ADVANCED_FACE ( 'NONE', ( #8595 ), #3875, .T. ) ;
#12051 =( LENGTH_UNIT ( ) NAMED_UNIT ( * ) SI_UNIT ( .MILLI., .METRE. ) );
#12052 = DIRECTION ( 'NONE',  ( 0.000000000000000000, -1.000000000000000000, 0.000000000000000000 ) ) ;
#12053 = ORIENTED_EDGE ( 'NONE', *, *, #10213, .F. ) ;
#12054 = AXIS2_PLACEMENT_3D ( 'NONE', #6151, #15636, #12521 ) ;
#12055 = EDGE_CURVE ( 'NONE', #5899, #3093, #18164, .T. ) ;
#12056 = VERTEX_POINT ( 'NONE', #6969 ) ;
#12057 = ADVANCED_FACE ( 'NONE', ( #5520 ), #19504, .T. ) ;
#12058 = VERTEX_POINT ( 'NONE', #13374 ) ;
#12059 = ORIENTED_EDGE ( 'NONE', *, *, #10249, .F. ) ;
#12060 = EDGE_CURVE ( 'NONE', #825, #6147, #14561, .T. ) ;
#12061 = CARTESIAN_POINT ( 'NONE',  ( -80.71807173247304945, 138.7734074251775667, 490.4856072914361107 ) ) ;
#12062 = AXIS2_PLACEMENT_3D ( 'NONE', #11131, #9796, #1847 ) ;
#12063 = CARTESIAN_POINT ( 'NONE',  ( 30.99999999999997868, 10.00000000000000000, -30.99999999999999645 ) ) ;
#12064 = DIRECTION ( 'NONE',  ( -0.000000000000000000, -1.000000000000000000, -0.000000000000000000 ) ) ;
#12065 = CARTESIAN_POINT ( 'NONE',  ( 55.48937290013659407, 209.7811923590224978, 348.0151256184570343 ) ) ;
#12066 = DIRECTION ( 'NONE',  ( 1.000000000000000000, 1.597771622610217359E-16, 0.000000000000000000 ) ) ;
#12067 = DIRECTION ( 'NONE',  ( 0.000000000000000000, 1.000000000000000000, 0.000000000000000000 ) ) ;
#12068 = DIRECTION ( 'NONE',  ( 1.000000000000000000, 5.889072920838430686E-16, -0.000000000000000000 ) ) ;
#12069 = CARTESIAN_POINT ( 'NONE',  ( 53.48937290013659407, 129.7247684487574588, 281.6050404526570219 ) ) ;
#12070 = DIRECTION ( 'NONE',  ( 0.000000000000000000, 1.000000000000000000, -0.000000000000000000 ) ) ;
#12071 = FACE_BOUND ( 'NONE', #600, .T. ) ;
#12072 = FACE_OUTER_BOUND ( 'NONE', #10670, .T. ) ;
#12073 = EDGE_CURVE ( 'NONE', #7788, #345, #400, .T. ) ;
#12074 = VERTEX_POINT ( 'NONE', #10497 ) ;
#12075 = ADVANCED_FACE ( 'NONE', ( #4319 ), #1191, .F. ) ;
#12076 = DIRECTION ( 'NONE',  ( 0.000000000000000000, 1.000000000000000000, 0.000000000000000000 ) ) ;
#12077 = ORIENTED_EDGE ( 'NONE', *, *, #7208, .T. ) ;
#12078 = ORIENTED_EDGE ( 'NONE', *, *, #19600, .F. ) ;
#12079 = CARTESIAN_POINT ( 'NONE',  ( 5.162501635565829972, 12.32407335584850117, 0.000000000000000000 ) ) ;
#12080 = EDGE_CURVE ( 'NONE', #6194, #10819, #1159, .T. ) ;
#12081 = DIRECTION ( 'NONE',  ( 0.000000000000000000, 0.000000000000000000, 1.000000000000000000 ) ) ;
#12082 = DIRECTION ( 'NONE',  ( 0.000000000000000000, 1.000000000000000000, 0.000000000000000000 ) ) ;
#12083 =( NAMED_UNIT ( * ) SI_UNIT ( $, .STERADIAN. ) SOLID_ANGLE_UNIT ( ) );
#12084 = PRESENTATION_STYLE_ASSIGNMENT (( #5989 ) ) ;
#12085 = CARTESIAN_POINT ( 'NONE',  ( -31.81980515339462912, 8.000000000000000000, -35.11980515339465114 ) ) ;
#12086 = PLANE ( 'NONE',  #505 ) ;
#12087 = LINE ( 'NONE', #18349, #5363 ) ;
#12088 = CARTESIAN_POINT ( 'NONE',  ( -80.27485217873301337, 138.9115877469687348, 489.2627155145635243 ) ) ;
#12089 = CARTESIAN_POINT ( 'NONE',  ( 463.8334540492693350, 214.2156642432025251, 250.0000000000000000 ) ) ;
#12090 = EDGE_LOOP ( 'NONE', ( #15206, #8579, #19403, #11898 ) ) ;
#12091 = SURFACE_SIDE_STYLE ('',( #5808 ) ) ;
#12092 = DIRECTION ( 'NONE',  ( 0.000000000000000000, -0.000000000000000000, -1.000000000000000000 ) ) ;
#12093 = EDGE_CURVE ( 'NONE', #5629, #2165, #2663, .T. ) ;
#12094 = AXIS2_PLACEMENT_3D ( 'NONE', #608, #5368, #8464 ) ;
#12095 = ORIENTED_EDGE ( 'NONE', *, *, #905, .T. ) ;
#12096 = ORIENTED_EDGE ( 'NONE', *, *, #14296, .T. ) ;
#12097 = PLANE ( 'NONE',  #17268 ) ;
#12098 = FACE_OUTER_BOUND ( 'NONE', #10867, .T. ) ;
#12099 = VERTEX_POINT ( 'NONE', #20060 ) ;
#12100 = SURFACE_STYLE_FILL_AREA ( #11800 ) ;
#12101 = STYLED_ITEM ( 'NONE', ( #16340 ), #11393 ) ;
#12102 = DIRECTION ( 'NONE',  ( 0.000000000000000000, 0.000000000000000000, 1.000000000000000000 ) ) ;
#12103 = CIRCLE ( 'NONE', #898, 10.00000000000000888 ) ;
#12104 = ORIENTED_EDGE ( 'NONE', *, *, #15402, .T. ) ;
#12105 = FACE_OUTER_BOUND ( 'NONE', #17585, .T. ) ;
#12106 = FACE_BOUND ( 'NONE', #19509, .T. ) ;
#12107 = SHAPE_DEFINITION_REPRESENTATION ( #9240, #13279 ) ;
#12108 = ORIENTED_EDGE ( 'NONE', *, *, #6729, .T. ) ;
#12109 = SURFACE_SIDE_STYLE ('',( #9118 ) ) ;
#12110 = VERTEX_POINT ( 'NONE', #5779 ) ;
#12111 = ORIENTED_EDGE ( 'NONE', *, *, #10506, .T. ) ;
#12112 = ORIENTED_EDGE ( 'NONE', *, *, #5348, .T. ) ;
#12113 = DIRECTION ( 'NONE',  ( 1.000000000000000000, 0.000000000000000000, 0.000000000000000000 ) ) ;
#12114 = ORIENTED_EDGE ( 'NONE', *, *, #6258, .F. ) ;
#12115 = DIRECTION ( 'NONE',  ( 1.000000000000000000, 0.000000000000000000, 0.000000000000000000 ) ) ;
#12116 = CARTESIAN_POINT ( 'NONE',  ( 31.00000000000001776, 0.000000000000000000, -25.99999999999999645 ) ) ;
#12117 = ORIENTED_EDGE ( 'NONE', *, *, #13428, .F. ) ;
#12118 =( LENGTH_UNIT ( ) NAMED_UNIT ( * ) SI_UNIT ( .MILLI., .METRE. ) );
#12119 = DIRECTION ( 'NONE',  ( 0.000000000000000000, 0.000000000000000000, -1.000000000000000000 ) ) ;
#12120 = CYLINDRICAL_SURFACE ( 'NONE', #2030, 5.000000000000004441 ) ;
#12121 = FACE_BOUND ( 'NONE', #2857, .T. ) ;
#12122 = CARTESIAN_POINT ( 'NONE',  ( 53.48937290013659407, 209.7811923590224978, 348.0151256184570343 ) ) ;
#12123 = CYLINDRICAL_SURFACE ( 'NONE', #15758, 1.000000000000000000 ) ;
#12124 = ADVANCED_FACE ( 'NONE', ( #5967 ), #8854, .F. ) ;
#12125 = LINE ( 'NONE', #10477, #15926 ) ;
#12126 = CARTESIAN_POINT ( 'NONE',  ( 30.90550859392664762, -60.11391548236647253, 66.87703344121202065 ) ) ;
#12127 = SURFACE_STYLE_FILL_AREA ( #2330 ) ;
#12128 = SURFACE_SIDE_STYLE ('',( #19941 ) ) ;
#12129 = CARTESIAN_POINT ( 'NONE',  ( 0.000000000000000000, 145.9162550801369491, -97.94896630388704750 ) ) ;
#12130 = PRESENTATION_LAYER_ASSIGNMENT (  '', '', ( #20352 ) ) ;
#12131 = CARTESIAN_POINT ( 'NONE',  ( 0.000000000000000000, 0.000000000000000000, 250.0000000000000000 ) ) ;
#12132 = LINE ( 'NONE', #16991, #2276 ) ;
#12133 = ORIENTED_EDGE ( 'NONE', *, *, #1534, .F. ) ;
#12134 = ORIENTED_EDGE ( 'NONE', *, *, #859, .F. ) ;
#12135 = ADVANCED_FACE ( 'NONE', ( #12149 ), #12245, .T. ) ;
#12136 = ORIENTED_EDGE ( 'NONE', *, *, #19762, .T. ) ;
#12137 = FACE_BOUND ( 'NONE', #12641, .T. ) ;
#12138 = ORIENTED_EDGE ( 'NONE', *, *, #6579, .F. ) ;
#12139 = CARTESIAN_POINT ( 'NONE',  ( -1.000000000000014655, 152.4824555358011082, 486.3411705753778165 ) ) ;
#12140 = VECTOR ( 'NONE', #14618, 1000.000000000000000 ) ;
#12141 = DIRECTION ( 'NONE',  ( -1.000000000000000000, 0.000000000000000000, 0.000000000000000000 ) ) ;
#12142 = EDGE_CURVE ( 'NONE', #16530, #12468, #11053, .T. ) ;
#12143 = COLOUR_RGB ( '', 0.09019608, 0.27058824, 0.51372549) ;
#12144 = ORIENTED_EDGE ( 'NONE', *, *, #1906, .F. ) ;
#12145 = CARTESIAN_POINT ( 'NONE',  ( -30.99999999999999289, 0.000000000000000000, 31.00000000000000000 ) ) ;
#12146 = LINE ( 'NONE', #5777, #3175 ) ;
#12147 = EDGE_CURVE ( 'NONE', #18810, #17220, #20371, .T. ) ;
#12148 = CARTESIAN_POINT ( 'NONE',  ( 0.000000000000000000, 3.000000000000000000, 0.000000000000000000 ) ) ;
#12149 = FACE_OUTER_BOUND ( 'NONE', #17255, .T. ) ;
#12150 = DIRECTION ( 'NONE',  ( -1.000000000000000000, 0.000000000000000000, 3.854941057726254367E-16 ) ) ;
#12151 = DIRECTION ( 'NONE',  ( -1.000000000000000000, 0.000000000000000000, -1.734723475976807094E-15 ) ) ;
#12152 = EDGE_CURVE ( 'NONE', #4285, #4676, #6731, .T. ) ;
#12153 = LINE ( 'NONE', #18528, #6292 ) ;
#12154 = PLANE ( 'NONE',  #42 ) ;
#12155 = CARTESIAN_POINT ( 'NONE',  ( 30.99999999999997868, 0.000000000000000000, -30.99999999999999645 ) ) ;
#12156 = EDGE_CURVE ( 'NONE', #3178, #5105, #9159, .T. ) ;
#12157 = VECTOR ( 'NONE', #13193, 1000.000000000000000 ) ;
#12158 =( GEOMETRIC_REPRESENTATION_CONTEXT ( 3 ) GLOBAL_UNCERTAINTY_ASSIGNED_CONTEXT ( ( #11838 ) ) GLOBAL_UNIT_ASSIGNED_CONTEXT ( ( #12358, #15358, #7818 ) ) REPRESENTATION_CONTEXT ( 'NONE', 'WORKASPACE' ) );
#12159 = MECHANICAL_DESIGN_GEOMETRIC_PRESENTATION_REPRESENTATION (  '', ( #10169 ), #5568 ) ;
#12160 = AXIS2_PLACEMENT_3D ( 'NONE', #2934, #9330, #4388 ) ;
#12161 = ORIENTED_EDGE ( 'NONE', *, *, #1427, .F. ) ;
#12162 = ORIENTED_EDGE ( 'NONE', *, *, #8431, .F. ) ;
#12163 = EDGE_CURVE ( 'NONE', #12183, #20011, #10009, .T. ) ;
#12164 = EDGE_LOOP ( 'NONE', ( #1334, #8347, #11807, #6914 ) ) ;
#12165 = ORIENTED_EDGE ( 'NONE', *, *, #14371, .T. ) ;
#12166 = UNCERTAINTY_MEASURE_WITH_UNIT (LENGTH_MEASURE( 1.000000000000000082E-05 ), #17635, 'distance_accuracy_value', 'NONE');
#12167 = FACE_OUTER_BOUND ( 'NONE', #19639, .T. ) ;
#12168 = VECTOR ( 'NONE', #9958, 1000.000000000000000 ) ;
#12169 = FACE_OUTER_BOUND ( 'NONE', #4641, .T. ) ;
#12170 = DIRECTION ( 'NONE',  ( 0.000000000000000000, -0.000000000000000000, 1.000000000000000000 ) ) ;
#12171 = AXIS2_PLACEMENT_3D ( 'NONE', #2512, #15088, #19497 ) ;
#12172 = CARTESIAN_POINT ( 'NONE',  ( -34.99999999999996447, 0.000000000000000000, -40.00000000000000711 ) ) ;
#12173 = DIRECTION ( 'NONE',  ( 1.000000000000000000, 0.000000000000000000, 0.000000000000000000 ) ) ;
#12174 = CARTESIAN_POINT ( 'NONE',  ( -81.18192946989242387, 139.7703989349477354, 490.5655098180907885 ) ) ;
#12175 = CARTESIAN_POINT ( 'NONE',  ( -37.00000000000000000, 68.00000000000000000, -22.99999999999999645 ) ) ;
#12176 = EDGE_LOOP ( 'NONE', ( #14499, #20291, #3339, #11027 ) ) ;
#12177 = SURFACE_SIDE_STYLE ('',( #15387 ) ) ;
#12178 = CARTESIAN_POINT ( 'NONE',  ( 21.00000000000000000, 19.00000000000000000, -31.00000000000003908 ) ) ;
#12179 = DIRECTION ( 'NONE',  ( 1.000000000000000000, -0.000000000000000000, 0.000000000000000000 ) ) ;
#12180 = VECTOR ( 'NONE', #9746, 1000.000000000000000 ) ;
#12181 = VECTOR ( 'NONE', #9916, 1000.000000000000000 ) ;
#12182 = ORIENTED_EDGE ( 'NONE', *, *, #15982, .F. ) ;
#12183 = VERTEX_POINT ( 'NONE', #19020 ) ;
#12184 = EDGE_CURVE ( 'NONE', #584, #792, #3182, .T. ) ;
#12185 = LINE ( 'NONE', #10641, #13334 ) ;
#12186 = SURFACE_STYLE_USAGE ( .BOTH. , #2701 ) ;
#12187 = ORIENTED_EDGE ( 'NONE', *, *, #11550, .F. ) ;
#12188 = FACE_OUTER_BOUND ( 'NONE', #7977, .T. ) ;
#12189 = VECTOR ( 'NONE', #11260, 1000.000000000000000 ) ;
#12190 = CARTESIAN_POINT ( 'NONE',  ( -80.99999999999995737, 140.4048636633015406, 500.8237260975782874 ) ) ;
#12191 = AXIS2_PLACEMENT_3D ( 'NONE', #10949, #320, #16027 ) ;
#12192 = DIRECTION ( 'NONE',  ( 0.000000000000000000, 0.000000000000000000, -1.000000000000000000 ) ) ;
#12193 = VECTOR ( 'NONE', #14863, 1000.000000000000000 ) ;
#12194 = CARTESIAN_POINT ( 'NONE',  ( 30.99999999999999645, 3.000000000000000000, 26.00000000000000355 ) ) ;
#12195 = ORIENTED_EDGE ( 'NONE', *, *, #9379, .F. ) ;
#12196 = CARTESIAN_POINT ( 'NONE',  ( 178.4893729001365443, 0.000000000000000000, -97.94896630388704750 ) ) ;
#12197 = PLANE ( 'NONE',  #11888 ) ;
#12198 = DIRECTION ( 'NONE',  ( 0.000000000000000000, -1.000000000000000000, 0.000000000000000000 ) ) ;
#12199 = SHAPE_DEFINITION_REPRESENTATION ( #17141, #12483 ) ;
#12200 = ORIENTED_EDGE ( 'NONE', *, *, #14435, .T. ) ;
#12201 = VERTEX_POINT ( 'NONE', #14308 ) ;
#12202 = DIRECTION ( 'NONE',  ( 0.000000000000000000, 0.000000000000000000, -1.000000000000000000 ) ) ;
#12203 = ORIENTED_EDGE ( 'NONE', *, *, #13166, .F. ) ;
#12204 = ORIENTED_EDGE ( 'NONE', *, *, #16568, .T. ) ;
#12205 = EDGE_LOOP ( 'NONE', ( #5110, #16398, #5704, #12973 ) ) ;
#12206 = VECTOR ( 'NONE', #15775, 1000.000000000000000 ) ;
#12207 = MECHANICAL_DESIGN_GEOMETRIC_PRESENTATION_REPRESENTATION (  '', ( #2997 ), #19121 ) ;
#12208 = LINE ( 'NONE', #5837, #15001 ) ;
#12209 = ORIENTED_EDGE ( 'NONE', *, *, #5479, .T. ) ;
#12210 = DIRECTION ( 'NONE',  ( 0.000000000000000000, 0.000000000000000000, -1.000000000000000000 ) ) ;
#12211 = CARTESIAN_POINT ( 'NONE',  ( -1.000000000000000888, 152.4824555358010798, 510.3921618609452935 ) ) ;
#12212 =( NAMED_UNIT ( * ) SI_UNIT ( $, .STERADIAN. ) SOLID_ANGLE_UNIT ( ) );
#12213 = FACE_OUTER_BOUND ( 'NONE', #9148, .T. ) ;
#12214 = CARTESIAN_POINT ( 'NONE',  ( -44.50085094405410757, 209.4098724938429541, 505.3921618609452935 ) ) ;
#12215 = CARTESIAN_POINT ( 'NONE',  ( 21.00000000000000000, 8.000000000000000000, -35.00000000000000711 ) ) ;
#12216 = ADVANCED_FACE ( 'NONE', ( #10710 ), #6384, .F. ) ;
#12217 = FILL_AREA_STYLE ('',( #2433 ) ) ;
#12218 = DIRECTION ( 'NONE',  ( -0.000000000000000000, -0.000000000000000000, 1.000000000000000000 ) ) ;
#12219 = DIRECTION ( 'NONE',  ( 0.000000000000000000, 0.000000000000000000, -1.000000000000000000 ) ) ;
#12220 = STYLED_ITEM ( 'NONE', ( #13259 ), #17761 ) ;
#12221 = CARTESIAN_POINT ( 'NONE',  ( 133.4893729001365728, 0.000000000000000000, 0.000000000000000000 ) ) ;
#12222 = DIRECTION ( 'NONE',  ( 1.000000000000000000, 0.000000000000000000, 0.000000000000000000 ) ) ;
#12223 = DIRECTION ( 'NONE',  ( -0.000000000000000000, -1.000000000000000000, 0.000000000000000000 ) ) ;
#12224 = CARTESIAN_POINT ( 'NONE',  ( -31.00000000000001776, 10.00000000000000000, 31.00000000000000000 ) ) ;
#12225 = SURFACE_STYLE_USAGE ( .BOTH. , #8931 ) ;
#12226 = AXIS2_PLACEMENT_3D ( 'NONE', #13267, #671, #14598 ) ;
#12227 = DIRECTION ( 'NONE',  ( 0.000000000000000000, 0.000000000000000000, -1.000000000000000000 ) ) ;
#12228 = VERTEX_POINT ( 'NONE', #1827 ) ;
#12229 = ORIENTED_EDGE ( 'NONE', *, *, #16119, .T. ) ;
#12230 = ORIENTED_EDGE ( 'NONE', *, *, #9116, .F. ) ;
#12231 = EDGE_LOOP ( 'NONE', ( #15240, #20346, #8933, #19397 ) ) ;
#12232 = ADVANCED_FACE ( 'NONE', ( #14502 ), #5339, .T. ) ;
#12233 = DIRECTION ( 'NONE',  ( -1.000000000000000000, -2.135044278125301096E-16, 0.000000000000000000 ) ) ;
#12234 = VECTOR ( 'NONE', #1973, 1000.000000000000000 ) ;
#12235 = ORIENTED_EDGE ( 'NONE', *, *, #7113, .F. ) ;
#12236 = LINE ( 'NONE', #4125, #19867 ) ;
#12237 =( NAMED_UNIT ( * ) SI_UNIT ( $, .STERADIAN. ) SOLID_ANGLE_UNIT ( ) );
#12238 = LINE ( 'NONE', #13785, #4086 ) ;
#12239 = STYLED_ITEM ( 'NONE', ( #6800 ), #8166 ) ;
#12240 = EDGE_LOOP ( 'NONE', ( #8468, #14774, #15058, #7712 ) ) ;
#12241 = FACE_OUTER_BOUND ( 'NONE', #15734, .T. ) ;
#12242 = CYLINDRICAL_SURFACE ( 'NONE', #3711, 3.300000000000011369 ) ;
#12243 = CARTESIAN_POINT ( 'NONE',  ( 5.950000000000000178, 12.65000000000000036, 0.000000000000000000 ) ) ;
#12244 =( NAMED_UNIT ( * ) PLANE_ANGLE_UNIT ( ) SI_UNIT ( $, .RADIAN. ) );
#12245 = PLANE ( 'NONE',  #6402 ) ;
#12246 = AXIS2_PLACEMENT_3D ( 'NONE', #17796, #874, #3893 ) ;
#12247 = FACE_OUTER_BOUND ( 'NONE', #20019, .T. ) ;
#12248 = DIRECTION ( 'NONE',  ( -0.000000000000000000, -0.000000000000000000, 1.000000000000000000 ) ) ;
#12249 = DIRECTION ( 'NONE',  ( -1.000000000000000000, -0.000000000000000000, -0.000000000000000000 ) ) ;
#12250 = EDGE_CURVE ( 'NONE', #8486, #6469, #16388, .T. ) ;
#12251 = FILL_AREA_STYLE ('',( #16905 ) ) ;
#12252 = CARTESIAN_POINT ( 'NONE',  ( 10.00000000000000000, 306.0487089519832011, -80.00000000000380851 ) ) ;
#12253 =( GEOMETRIC_REPRESENTATION_CONTEXT ( 3 ) GLOBAL_UNCERTAINTY_ASSIGNED_CONTEXT ( ( #12381 ) ) GLOBAL_UNIT_ASSIGNED_CONTEXT ( ( #7295, #15122, #14921 ) ) REPRESENTATION_CONTEXT ( 'NONE', 'WORKASPACE' ) );
#12254 = ORIENTED_EDGE ( 'NONE', *, *, #6628, .T. ) ;
#12255 = EDGE_CURVE ( 'NONE', #10724, #566, #2131, .T. ) ;
#12256 = AXIS2_PLACEMENT_3D ( 'NONE', #6156, #9626, #12631 ) ;
#12257 = ORIENTED_EDGE ( 'NONE', *, *, #3120, .F. ) ;
#12258 = ORIENTED_EDGE ( 'NONE', *, *, #8489, .T. ) ;
#12259 = AXIS2_PLACEMENT_3D ( 'NONE', #7686, #7990, #20255 ) ;
#12260 = EDGE_LOOP ( 'NONE', ( #14323, #6603, #9726, #15806 ) ) ;
#12261 = CIRCLE ( 'NONE', #15581, 10.00000000000000888 ) ;
#12262 = ORIENTED_EDGE ( 'NONE', *, *, #19885, .T. ) ;
#12263 = CARTESIAN_POINT ( 'NONE',  ( 34.00000000000002842, -20.00000000000000000, 23.00000000000000355 ) ) ;
#12264 = EDGE_CURVE ( 'NONE', #17965, #18122, #3385, .T. ) ;
#12265 = DIRECTION ( 'NONE',  ( -1.000000000000000000, -0.000000000000000000, -0.000000000000000000 ) ) ;
#12266 = CARTESIAN_POINT ( 'NONE',  ( 0.000000000000000000, 80.91625508013694912, 250.0000000000000000 ) ) ;
#12267 = EDGE_CURVE ( 'NONE', #8092, #7872, #3087, .T. ) ;
#12268 = VECTOR ( 'NONE', #14756, 1000.000000000000000 ) ;
#12269 = AXIS2_PLACEMENT_3D ( 'NONE', #7399, #12334, #20036 ) ;
#12270 = CARTESIAN_POINT ( 'NONE',  ( -31.00000000000005329, 10.00000000000000000, 26.00000000000000000 ) ) ;
#12271 = VECTOR ( 'NONE', #12006, 1000.000000000000000 ) ;
#12272 = CARTESIAN_POINT ( 'NONE',  ( 178.4893729001365728, 113.1299228374914918, 29.36128450348865471 ) ) ;
#12273 = CARTESIAN_POINT ( 'NONE',  ( 111.4893729001366012, 129.7247684487574588, 370.0000000000000000 ) ) ;
#12274 = DIRECTION ( 'NONE',  ( -1.000000000000000000, 0.000000000000000000, 0.000000000000000000 ) ) ;
#12275 = CARTESIAN_POINT ( 'NONE',  ( 0.8442384278957183463, 139.4861549369088038, 500.2186618848268722 ) ) ;
#12276 = ADVANCED_FACE ( 'NONE', ( #12983 ), #13186, .T. ) ;
#12277 = CLOSED_SHELL ( 'NONE', ( #18329, #418, #11116, #12040, #6305, #3492, #1705, #18050, #12428, #3479, #9595, #2057 ) ) ;
#12278 = VERTEX_POINT ( 'NONE', #17703 ) ;
#12279 = SURFACE_STYLE_USAGE ( .BOTH. , #12177 ) ;
#12280 = CIRCLE ( 'NONE', #8009, 10.00000000000000888 ) ;
#12281 = AXIS2_PLACEMENT_3D ( 'NONE', #17218, #105, #18553 ) ;
#12282 = EDGE_CURVE ( 'NONE', #13880, #3979, #8521, .T. ) ;
#12283 = ORIENTED_EDGE ( 'NONE', *, *, #6729, .F. ) ;
#12284 = EDGE_CURVE ( 'NONE', #13028, #9760, #6588, .T. ) ;
#12285 = DIRECTION ( 'NONE',  ( 0.000000000000000000, 0.000000000000000000, -1.000000000000000000 ) ) ;
#12286 = MECHANICAL_DESIGN_GEOMETRIC_PRESENTATION_REPRESENTATION (  '', ( #10004 ), #6726 ) ;
#12287 = ORIENTED_EDGE ( 'NONE', *, *, #17099, .T. ) ;
#12288 = CARTESIAN_POINT ( 'NONE',  ( -1.450371633464476962E-15, 152.4824555358010798, 509.3921618609452935 ) ) ;
#12289 = DIRECTION ( 'NONE',  ( 0.000000000000000000, 0.000000000000000000, -1.000000000000000000 ) ) ;
#12290 = VERTEX_POINT ( 'NONE', #11424 ) ;
#12291 =( NAMED_UNIT ( * ) PLANE_ANGLE_UNIT ( ) SI_UNIT ( $, .RADIAN. ) );
#12292 =( NAMED_UNIT ( * ) PLANE_ANGLE_UNIT ( ) SI_UNIT ( $, .RADIAN. ) );
#12293 = AXIS2_PLACEMENT_3D ( 'NONE', #2013, #9661, #6901 ) ;
#12294 = MECHANICAL_DESIGN_GEOMETRIC_PRESENTATION_REPRESENTATION (  '', ( #4066 ), #18206 ) ;
#12295 = CARTESIAN_POINT ( 'NONE',  ( -79.99999999999995737, 141.6406393683236331, 501.8237260975782874 ) ) ;
#12296 = CARTESIAN_POINT ( 'NONE',  ( 4.469960816887838430E-15, 26.00000000000000000, 36.50000000000000000 ) ) ;
#12297 = EDGE_LOOP ( 'NONE', ( #15523, #14475, #5081, #3604, #13221, #2594, #7007, #10932, #9959, #9354, #18078, #6061, #5145, #20221, #11493, #18537 ) ) ;
#12298 = FACE_OUTER_BOUND ( 'NONE', #2873, .T. ) ;
#12299 = FACE_OUTER_BOUND ( 'NONE', #3168, .T. ) ;
#12300 = DIRECTION ( 'NONE',  ( 0.000000000000000000, 0.000000000000000000, 1.000000000000000000 ) ) ;
#12301 = APPLICATION_PROTOCOL_DEFINITION ( 'draft international standard', 'automotive_design', 1998, #16595 ) ;
#12302 = MECHANICAL_DESIGN_GEOMETRIC_PRESENTATION_REPRESENTATION (  '', ( #15285 ), #16615 ) ;
#12303 = COLOUR_RGB ( '', 0.40784314, 0.44705882, 0.49803922) ;
#12304 = CARTESIAN_POINT ( 'NONE',  ( -58.16843972078500258, 319.7545334744432353, 481.2863735482146126 ) ) ;
#12305 = EDGE_CURVE ( 'NONE', #13028, #6572, #3761, .T. ) ;
#12306 = ORIENTED_EDGE ( 'NONE', *, *, #9116, .T. ) ;
#12307 = VECTOR ( 'NONE', #5309, 1000.000000000000000 ) ;
#12308 = VERTEX_POINT ( 'NONE', #16086 ) ;
#12309 = ORIENTED_EDGE ( 'NONE', *, *, #3852, .F. ) ;
#12310 = EDGE_CURVE ( 'NONE', #3441, #593, #681, .T. ) ;
#12311 = AXIS2_PLACEMENT_3D ( 'NONE', #15649, #6256, #1576 ) ;
#12312 = COLOUR_RGB ( '', 0.08235294, 0.09019608, 0.10196078) ;
#12313 = AXIS2_PLACEMENT_3D ( 'NONE', #10735, #18253, #2493 ) ;
#12314 = PLANE ( 'NONE',  #2800 ) ;
#12315 = CIRCLE ( 'NONE', #126, 1.000000000000000888 ) ;
#12316 = ORIENTED_EDGE ( 'NONE', *, *, #8145, .T. ) ;
#12317 = LINE ( 'NONE', #13972, #3756 ) ;
#12318 = EDGE_CURVE ( 'NONE', #1517, #1728, #11518, .T. ) ;
#12319 = ORIENTED_EDGE ( 'NONE', *, *, #4583, .F. ) ;
#12320 = DIRECTION ( 'NONE',  ( 1.000000000000000000, -0.000000000000000000, -0.000000000000000000 ) ) ;
#12321 = AXIS2_PLACEMENT_3D ( 'NONE', #8971, #15068, #8787 ) ;
#12322 = DIRECTION ( 'NONE',  ( -0.000000000000000000, -1.000000000000000000, 0.000000000000000000 ) ) ;
#12323 = STYLED_ITEM ( 'NONE', ( #18488 ), #930 ) ;
#12324 = DIRECTION ( 'NONE',  ( 1.000000000000000000, 0.000000000000000000, 0.000000000000000000 ) ) ;
#12325 = PRESENTATION_LAYER_ASSIGNMENT (  '', '', ( #15645 ) ) ;
#12326 = SURFACE_SIDE_STYLE ('',( #18390 ) ) ;
#12327 = DIRECTION ( 'NONE',  ( -0.000000000000000000, 1.000000000000000000, -0.000000000000000000 ) ) ;
#12328 = CYLINDRICAL_SURFACE ( 'NONE', #12160, 5.000000000000004441 ) ;
#12329 = CYLINDRICAL_SURFACE ( 'NONE', #13002, 3.283624802691453848 ) ;
#12330 = CARTESIAN_POINT ( 'NONE',  ( 153.4893729001366864, 113.1299228374914634, 220.6387154965113382 ) ) ;
#12331 = AXIS2_PLACEMENT_3D ( 'NONE', #6642, #3328, #8390 ) ;
#12332 = VECTOR ( 'NONE', #410, 1000.000000000000000 ) ;
#12333 = SURFACE_STYLE_FILL_AREA ( #18709 ) ;
#12334 = DIRECTION ( 'NONE',  ( 0.000000000000000000, 0.000000000000000000, 1.000000000000000000 ) ) ;
#12335 = DIRECTION ( 'NONE',  ( 0.000000000000000000, 0.000000000000000000, 1.000000000000000000 ) ) ;
#12337 = AXIS2_PLACEMENT_3D ( 'NONE', #4104, #5853, #10478 ) ;
#12336 = CARTESIAN_POINT ( 'NONE',  ( 30.99999999999997868, 0.000000000000000000, -30.99999999999999645 ) ) ;
#12338 = DIRECTION ( 'NONE',  ( -0.000000000000000000, -1.000000000000000000, 0.000000000000000000 ) ) ;
#12339 = AXIS2_PLACEMENT_3D ( 'NONE', #4141, #18529, #4235 ) ;
#12340 = SURFACE_SIDE_STYLE ('',( #7699 ) ) ;
#12341 = DIRECTION ( 'NONE',  ( -1.000000000000000000, -0.000000000000000000, -0.000000000000000000 ) ) ;
#12342 = ORIENTED_EDGE ( 'NONE', *, *, #13087, .T. ) ;
#12343 = VECTOR ( 'NONE', #17735, 1000.000000000000000 ) ;
#12344 = VERTEX_POINT ( 'NONE', #11308 ) ;
#12345 = CIRCLE ( 'NONE', #1793, 5.000000000000000888 ) ;
#12346 = ORIENTED_EDGE ( 'NONE', *, *, #9222, .T. ) ;
#12347 = EDGE_CURVE ( 'NONE', #13802, #886, #14809, .T. ) ;
#12348 = ORIENTED_EDGE ( 'NONE', *, *, #4995, .F. ) ;
#12349 = DIRECTION ( 'NONE',  ( -0.000000000000000000, 0.000000000000000000, 1.000000000000000000 ) ) ;
#12350 = VECTOR ( 'NONE', #7923, 1000.000000000000000 ) ;
#12351 = FACE_OUTER_BOUND ( 'NONE', #9212, .T. ) ;
#12352 = AXIS2_PLACEMENT_3D ( 'NONE', #19940, #8624, #10388 ) ;
#12353 = EDGE_LOOP ( 'NONE', ( #7604, #5350, #7365, #14782 ) ) ;
#12354 = CARTESIAN_POINT ( 'NONE',  ( -3.795335389125411904E-15, 146.8256012863087676, 480.6843163258853906 ) ) ;
#12355 = AXIS2_PLACEMENT_3D ( 'NONE', #11087, #3158, #14170 ) ;
#12356 = SURFACE_SIDE_STYLE ('',( #18634 ) ) ;
#12357 = ORIENTED_EDGE ( 'NONE', *, *, #16373, .T. ) ;
#12358 =( LENGTH_UNIT ( ) NAMED_UNIT ( * ) SI_UNIT ( .MILLI., .METRE. ) );
#12359 = DIRECTION ( 'NONE',  ( 0.000000000000000000, 1.000000000000000000, 0.000000000000000000 ) ) ;
#12360 =( GEOMETRIC_REPRESENTATION_CONTEXT ( 3 ) GLOBAL_UNCERTAINTY_ASSIGNED_CONTEXT ( ( #19182 ) ) GLOBAL_UNIT_ASSIGNED_CONTEXT ( ( #20317, #10955, #1546 ) ) REPRESENTATION_CONTEXT ( 'NONE', 'WORKASPACE' ) );
#12361 = CARTESIAN_POINT ( 'NONE',  ( 18.99999999999998224, 8.000000000000000000, -39.99999999999999289 ) ) ;
#12362 = ORIENTED_EDGE ( 'NONE', *, *, #12915, .F. ) ;
#12363 =( NAMED_UNIT ( * ) PLANE_ANGLE_UNIT ( ) SI_UNIT ( $, .RADIAN. ) );
#12364 =( NAMED_UNIT ( * ) PLANE_ANGLE_UNIT ( ) SI_UNIT ( $, .RADIAN. ) );
#12365 = AXIS2_PLACEMENT_3D ( 'NONE', #15107, #16770, #955 ) ;
#12366 = CARTESIAN_POINT ( 'NONE',  ( 32.99999999999998579, 8.000000000000000000, 25.99999999999999645 ) ) ;
#12367 = FACE_OUTER_BOUND ( 'NONE', #13158, .T. ) ;
#12368 = LINE ( 'NONE', #8311, #17470 ) ;
#12369 = LINE ( 'NONE', #19868, #7949 ) ;
#12370 = APPLICATION_CONTEXT ( 'automotive_design' ) ;
#12371 = ADVANCED_FACE ( 'NONE', ( #6806 ), #19133, .F. ) ;
#12372 = ORIENTED_EDGE ( 'NONE', *, *, #8450, .T. ) ;
#12373 = VERTEX_POINT ( 'NONE', #19936 ) ;
#12374 = VERTEX_POINT ( 'NONE', #5538 ) ;
#12375 = ORIENTED_EDGE ( 'NONE', *, *, #1390, .T. ) ;
#12376 = ORIENTED_EDGE ( 'NONE', *, *, #14322, .T. ) ;
#12377 = ORIENTED_EDGE ( 'NONE', *, *, #19336, .T. ) ;
#12378 = DIRECTION ( 'NONE',  ( 0.000000000000000000, 0.000000000000000000, 1.000000000000000000 ) ) ;
#12379 = VECTOR ( 'NONE', #17717, 1000.000000000000000 ) ;
#12380 = FACE_OUTER_BOUND ( 'NONE', #8847, .T. ) ;
#12381 = UNCERTAINTY_MEASURE_WITH_UNIT (LENGTH_MEASURE( 1.000000000000000082E-05 ), #7295, 'distance_accuracy_value', 'NONE');
#12382 = EDGE_CURVE ( 'NONE', #18726, #15525, #9663, .T. ) ;
#12383 = CARTESIAN_POINT ( 'NONE',  ( 53.48937290013658696, 119.5973956464515879, 322.0399576098686225 ) ) ;
#12384 = PRESENTATION_STYLE_ASSIGNMENT (( #20085 ) ) ;
#12385 = DIRECTION ( 'NONE',  ( 0.000000000000000000, 0.000000000000000000, 1.000000000000000000 ) ) ;
#12386 = PRODUCT_DEFINITION_SHAPE ( 'NONE', 'NONE',  #8109 ) ;
#12387 = CARTESIAN_POINT ( 'NONE',  ( 25.99999999999998224, 8.000000000000000000, -32.99999999999999289 ) ) ;
#12388 = PRODUCT_RELATED_PRODUCT_CATEGORY ( 'part', '', ( #15518 ) ) ;
#12389 = CARTESIAN_POINT ( 'NONE',  ( 178.4893729001365728, 103.1299228374914776, 170.4174721992565082 ) ) ;
#12390 = PRESENTATION_STYLE_ASSIGNMENT (( #104 ) ) ;
#12391 = SURFACE_SIDE_STYLE ('',( #1533 ) ) ;
#12392 = EDGE_LOOP ( 'NONE', ( #3230, #10509, #14483, #1412 ) ) ;
#12393 = DIRECTION ( 'NONE',  ( 1.000000000000000000, 0.000000000000000000, 0.000000000000000000 ) ) ;
#12394 = CARTESIAN_POINT ( 'NONE',  ( -38.50085094405407204, 175.4489062796178871, 505.3921618609452935 ) ) ;
#12395 = EDGE_CURVE ( 'NONE', #10424, #7147, #2738, .T. ) ;
#12396 = DIRECTION ( 'NONE',  ( 0.000000000000000000, 0.000000000000000000, 1.000000000000000000 ) ) ;
#12397 = MECHANICAL_DESIGN_GEOMETRIC_PRESENTATION_REPRESENTATION (  '', ( #1171 ), #11077 ) ;
#12398 = EDGE_CURVE ( 'NONE', #10613, #19303, #10576, .T. ) ;
#12399 = VERTEX_POINT ( 'NONE', #8621 ) ;
#12400 = EDGE_CURVE ( 'NONE', #2165, #10613, #10331, .T. ) ;
#12401 = EDGE_CURVE ( 'NONE', #53, #17182, #18395, .T. ) ;
#12402 =( NAMED_UNIT ( * ) PLANE_ANGLE_UNIT ( ) SI_UNIT ( $, .RADIAN. ) );
#12403 = VERTEX_POINT ( 'NONE', #10270 ) ;
#12404 = CARTESIAN_POINT ( 'NONE',  ( 78.48937290013660117, 145.9162550801369491, 250.0000000000000000 ) ) ;
#12405 = DIRECTION ( 'NONE',  ( -0.000000000000000000, -1.000000000000000000, -0.000000000000000000 ) ) ;
#12406 = CIRCLE ( 'NONE', #16052, 18.50000000000000000 ) ;
#12407 = ORIENTED_EDGE ( 'NONE', *, *, #13913, .T. ) ;
#12408 = PLANE ( 'NONE',  #1813 ) ;
#12409 = DIRECTION ( 'NONE',  ( -0.000000000000000000, -1.000000000000000000, -0.000000000000000000 ) ) ;
#12410 = DIRECTION ( 'NONE',  ( 0.000000000000000000, 0.000000000000000000, -1.000000000000000000 ) ) ;
#12411 = EDGE_CURVE ( 'NONE', #4616, #19512, #11733, .T. ) ;
#12412 = DIRECTION ( 'NONE',  ( -1.000000000000000000, 0.000000000000000000, 7.715811803773179210E-14 ) ) ;
#12413 = EDGE_CURVE ( 'NONE', #7981, #6644, #13680, .T. ) ;
#12414 = DIRECTION ( 'NONE',  ( -1.000000000000000000, -9.815121534730717399E-17, 0.000000000000000000 ) ) ;
#12415 = CARTESIAN_POINT ( 'NONE',  ( 40.00000000000001421, 5.000000000000000888, -150.0000000000000000 ) ) ;
#12416 = VERTEX_POINT ( 'NONE', #10474 ) ;
#12417 = CARTESIAN_POINT ( 'NONE',  ( 35.99999999999999289, 6.000000000000000000, 17.99999999999998934 ) ) ;
#12418 = CARTESIAN_POINT ( 'NONE',  ( 31.00000000000001776, 10.00000000000000000, -25.99999999999999645 ) ) ;
#12419 = PLANE ( 'NONE',  #14612 ) ;
#12420 = SHAPE_DEFINITION_REPRESENTATION ( #3335, #1922 ) ;
#12421 = EDGE_LOOP ( 'NONE', ( #18926, #13226 ) ) ;
#12422 =( LENGTH_UNIT ( ) NAMED_UNIT ( * ) SI_UNIT ( .MILLI., .METRE. ) );
#12423 = ADVANCED_FACE ( 'NONE', ( #15333 ), #19631, .F. ) ;
#12424 = VERTEX_POINT ( 'NONE', #10383 ) ;
#12425 = ORIENTED_EDGE ( 'NONE', *, *, #16469, .T. ) ;
#12426 = VERTEX_POINT ( 'NONE', #3988 ) ;
#12427 = DIRECTION ( 'NONE',  ( 1.000000000000000000, 0.000000000000000000, 0.000000000000000000 ) ) ;
#12428 = ADVANCED_FACE ( 'NONE', ( #4205 ), #16687, .T. ) ;
#12429 = VERTEX_POINT ( 'NONE', #13767 ) ;
#12430 = LINE ( 'NONE', #8918, #17988 ) ;
#12431 = CARTESIAN_POINT ( 'NONE',  ( -77.99033078109007988, 127.7247684487574304, 254.0000000000000000 ) ) ;
#12432 = CARTESIAN_POINT ( 'NONE',  ( 30.99999999999999645, 0.000000000000000000, 26.00000000000001066 ) ) ;
#12433 = CIRCLE ( 'NONE', #6191, 9.000000000000007105 ) ;
#12434 = LINE ( 'NONE', #13764, #4288 ) ;
#12435 = DIRECTION ( 'NONE',  ( 0.000000000000000000, 0.000000000000000000, -1.000000000000000000 ) ) ;
#12436 = DIRECTION ( 'NONE',  ( 1.000000000000000000, 0.000000000000000000, 0.000000000000000000 ) ) ;
#12437 = CYLINDRICAL_SURFACE ( 'NONE', #9825, 1.000000000000000888 ) ;
#12438 = EDGE_CURVE ( 'NONE', #12712, #19421, #7396, .T. ) ;
#12439 = CARTESIAN_POINT ( 'NONE',  ( 31.00000000000004263, 68.00000000000000000, -25.99999999999999645 ) ) ;
#12440 = LINE ( 'NONE', #13683, #6027 ) ;
#12441 = FACE_BOUND ( 'NONE', #5925, .T. ) ;
#12442 = DIRECTION ( 'NONE',  ( 0.000000000000000000, 0.000000000000000000, 1.000000000000000000 ) ) ;
#12443 = FACE_OUTER_BOUND ( 'NONE', #3676, .T. ) ;
#12444 = CIRCLE ( 'NONE', #6516, 8.000000000000007105 ) ;
#12445 = EDGE_LOOP ( 'NONE', ( #6218, #4553, #9022, #12614 ) ) ;
#12446 = EDGE_CURVE ( 'NONE', #16969, #1878, #7891, .T. ) ;
#12447 = VECTOR ( 'NONE', #12218, 1000.000000000000000 ) ;
#12448 = ORIENTED_EDGE ( 'NONE', *, *, #7392, .T. ) ;
#12449 = ORIENTED_EDGE ( 'NONE', *, *, #18592, .F. ) ;
#12450 = ORIENTED_EDGE ( 'NONE', *, *, #18854, .T. ) ;
#12451 = DIRECTION ( 'NONE',  ( 1.000000000000000000, 0.000000000000000000, -0.000000000000000000 ) ) ;
#12452 = FACE_BOUND ( 'NONE', #15500, .T. ) ;
#12453 = VERTEX_POINT ( 'NONE', #20031 ) ;
#12454 = DIRECTION ( 'NONE',  ( 0.000000000000000000, 1.000000000000000000, 0.000000000000000000 ) ) ;
#12455 = DIRECTION ( 'NONE',  ( 0.000000000000000000, 1.000000000000000000, 0.000000000000000000 ) ) ;
#12456 = ORIENTED_EDGE ( 'NONE', *, *, #11420, .T. ) ;
#12457 = PLANE ( 'NONE',  #15465 ) ;
#12458 = CARTESIAN_POINT ( 'NONE',  ( 31.00000000000001421, 0.000000000000000000, 25.99999999999999645 ) ) ;
#12459 = CARTESIAN_POINT ( 'NONE',  ( 35.99999999999999289, 10.00000000000000000, 18.99999999999999289 ) ) ;
#12460 = MECHANICAL_DESIGN_GEOMETRIC_PRESENTATION_REPRESENTATION (  '', ( #6884 ), #9158 ) ;
#12461 =( NAMED_UNIT ( * ) PLANE_ANGLE_UNIT ( ) SI_UNIT ( $, .RADIAN. ) );
#12462 = DIRECTION ( 'NONE',  ( 8.479266908829339085E-16, -1.000000000000000000, 0.000000000000000000 ) ) ;
#12463 = DIRECTION ( 'NONE',  ( -0.000000000000000000, -0.000000000000000000, 1.000000000000000000 ) ) ;
#12464 = PLANE ( 'NONE',  #3700 ) ;
#12465 = ADVANCED_FACE ( 'NONE', ( #17272 ), #12329, .F. ) ;
#12466 = CARTESIAN_POINT ( 'NONE',  ( -38.50085094405407204, 159.0821755739672483, 510.3921618609452935 ) ) ;
#12467 = DIRECTION ( 'NONE',  ( 0.000000000000000000, 0.000000000000000000, 1.000000000000000000 ) ) ;
#12468 = VERTEX_POINT ( 'NONE', #18613 ) ;
#12469 = VERTEX_POINT ( 'NONE', #17070 ) ;
#12470 = ORIENTED_EDGE ( 'NONE', *, *, #10277, .F. ) ;
#12471 = AXIS2_PLACEMENT_3D ( 'NONE', #16433, #9929, #3943 ) ;
#12472 = LINE ( 'NONE', #7734, #9368 ) ;
#12473 = ORIENTED_EDGE ( 'NONE', *, *, #2158, .F. ) ;
#12474 = ORIENTED_EDGE ( 'NONE', *, *, #12783, .T. ) ;
#12475 = ORIENTED_EDGE ( 'NONE', *, *, #12255, .T. ) ;
#12476 = FACE_OUTER_BOUND ( 'NONE', #14016, .T. ) ;
#12477 = CYLINDRICAL_SURFACE ( 'NONE', #3994, 10.00000000000000888 ) ;
#12478 = LINE ( 'NONE', #15700, #1972 ) ;
#12479 = PLANE ( 'NONE',  #12965 ) ;
#12480 = FACE_OUTER_BOUND ( 'NONE', #16489, .T. ) ;
#12481 = FACE_OUTER_BOUND ( 'NONE', #13201, .T. ) ;
#12482 = SURFACE_STYLE_USAGE ( .BOTH. , #4549 ) ;
#12483 = SHAPE_REPRESENTATION ( 'TAS-006', ( #4044, #6049, #16544, #7692, #8679, #19206, #10275, #1348, #1408 ), #13593 ) ;
#12484 = AXIS2_PLACEMENT_3D ( 'NONE', #1114, #18131, #4035 ) ;
#12485 = DIRECTION ( 'NONE',  ( 0.000000000000000000, 0.000000000000000000, -1.000000000000000000 ) ) ;
#12486 = CARTESIAN_POINT ( 'NONE',  ( 0.000000000000000000, -3.000000000000000888, 0.000000000000000000 ) ) ;
#12487 = EDGE_CURVE ( 'NONE', #19036, #19368, #9681, .T. ) ;
#12488 = ORIENTED_EDGE ( 'NONE', *, *, #14163, .T. ) ;
#12489 = CIRCLE ( 'NONE', #6902, 0.9999999999999964473 ) ;
#12490 = LINE ( 'NONE', #1853, #15637 ) ;
#12491 = DIRECTION ( 'NONE',  ( -3.854941057726253874E-16, 0.000000000000000000, -1.000000000000000000 ) ) ;
#12492 = ORIENTED_EDGE ( 'NONE', *, *, #19058, .T. ) ;
#12493 = AXIS2_PLACEMENT_3D ( 'NONE', #3285, #9562, #15878 ) ;
#12494 =( GEOMETRIC_REPRESENTATION_CONTEXT ( 3 ) GLOBAL_UNCERTAINTY_ASSIGNED_CONTEXT ( ( #2335 ) ) GLOBAL_UNIT_ASSIGNED_CONTEXT ( ( #7424, #13307, #11853 ) ) REPRESENTATION_CONTEXT ( 'NONE', 'WORKASPACE' ) );
#12495 = AXIS2_PLACEMENT_3D ( 'NONE', #12129, #2942, #1174 ) ;
#12496 = DIRECTION ( 'NONE',  ( -1.000000000000000000, -0.000000000000000000, -0.000000000000000000 ) ) ;
#12497 = ORIENTED_EDGE ( 'NONE', *, *, #4090, .F. ) ;
#12498 = EDGE_CURVE ( 'NONE', #12308, #8243, #1361, .T. ) ;
#12499 = CARTESIAN_POINT ( 'NONE',  ( 0.000000000000000000, 10.00000000000000000, -12.00000000000000178 ) ) ;
#12500 = EDGE_LOOP ( 'NONE', ( #16450, #1327, #14902, #1701 ) ) ;
#12501 = LINE ( 'NONE', #17130, #14976 ) ;
#12502 = CARTESIAN_POINT ( 'NONE',  ( 0.2098432949449543505, 140.7834779774802030, 501.2072179691460292 ) ) ;
#12503 = DIRECTION ( 'NONE',  ( 1.000000000000000000, 0.000000000000000000, 0.000000000000000000 ) ) ;
#12504 = FILL_AREA_STYLE ('',( #6533 ) ) ;
#12505 = FILL_AREA_STYLE_COLOUR ( '', #1781 ) ;
#12506 = ORIENTED_EDGE ( 'NONE', *, *, #9260, .T. ) ;
#12507 = DIRECTION ( 'NONE',  ( 0.000000000000000000, 1.000000000000000000, 0.000000000000000000 ) ) ;
#12508 = DIRECTION ( 'NONE',  ( 1.000000000000000000, 0.000000000000000000, 0.000000000000000000 ) ) ;
#12509 = CARTESIAN_POINT ( 'NONE',  ( 30.99999999999997513, 10.00000000000000000, 30.99999999999999645 ) ) ;
#12510 = VECTOR ( 'NONE', #2469, 1000.000000000000000 ) ;
#12511 = CONTEXT_DEPENDENT_SHAPE_REPRESENTATION ( #13693, #9765 ) ;
#12512 = EDGE_CURVE ( 'NONE', #13880, #9081, #20206, .T. ) ;
#12513 = AXIS2_PLACEMENT_3D ( 'NONE', #1860, #16125, #19471 ) ;
#12514 = ORIENTED_EDGE ( 'NONE', *, *, #18999, .F. ) ;
#12515 = VERTEX_POINT ( 'NONE', #5939 ) ;
#12516 = LINE ( 'NONE', #17252, #14872 ) ;
#12517 = ORIENTED_EDGE ( 'NONE', *, *, #16803, .F. ) ;
#12518 = ORIENTED_EDGE ( 'NONE', *, *, #8129, .T. ) ;
#12519 = EDGE_CURVE ( 'NONE', #12769, #7627, #14172, .T. ) ;
#12520 = ORIENTED_EDGE ( 'NONE', *, *, #13975, .F. ) ;
#12521 = DIRECTION ( 'NONE',  ( 0.000000000000000000, 1.000000000000000000, 0.000000000000000000 ) ) ;
#12522 = ORIENTED_EDGE ( 'NONE', *, *, #13349, .T. ) ;
#12523 = PRESENTATION_STYLE_ASSIGNMENT (( #15941 ) ) ;
#12524 = ORIENTED_EDGE ( 'NONE', *, *, #5140, .F. ) ;
#12525 = ADVANCED_FACE ( 'NONE', ( #11591 ), #3771, .T. ) ;
#12526 = AXIS2_PLACEMENT_3D ( 'NONE', #8656, #13505, #5560 ) ;
#12527 = DIRECTION ( 'NONE',  ( 0.000000000000000000, 0.000000000000000000, -1.000000000000000000 ) ) ;
#12528 = ADVANCED_FACE ( 'NONE', ( #157 ), #1798, .F. ) ;
#12529 = CYLINDRICAL_SURFACE ( 'NONE', #14569, 3.300000000000000711 ) ;
#12530 = DIRECTION ( 'NONE',  ( -0.000000000000000000, -1.000000000000000000, -0.000000000000000000 ) ) ;
#12531 = SURFACE_STYLE_FILL_AREA ( #15748 ) ;
#12532 = SURFACE_SIDE_STYLE ('',( #4502 ) ) ;
#12533 = ORIENTED_EDGE ( 'NONE', *, *, #680, .T. ) ;
#12534 = CARTESIAN_POINT ( 'NONE',  ( -77.99033078109007988, 127.7247684487574304, 357.7985149490353933 ) ) ;
#12535 = DIRECTION ( 'NONE',  ( -0.000000000000000000, -1.000000000000000000, -0.000000000000000000 ) ) ;
#12536 = CARTESIAN_POINT ( 'NONE',  ( 1.399999999999999911, 0.000000000000000000, 0.000000000000000000 ) ) ;
#12537 = CARTESIAN_POINT ( 'NONE',  ( -21.00000000000002842, 0.000000000000000000, -34.99999999999999289 ) ) ;
#12538 = EDGE_CURVE ( 'NONE', #10041, #4579, #6420, .T. ) ;
#12539 = CARTESIAN_POINT ( 'NONE',  ( 108.9893729001365870, 144.5787140289007766, 293.4524157190248275 ) ) ;
#12540 = FILL_AREA_STYLE_COLOUR ( '', #6927 ) ;
#12541 = VECTOR ( 'NONE', #12608, 1000.000000000000000 ) ;
#12542 = COLOUR_RGB ( '', 0.40784314, 0.44705882, 0.49803922) ;
#12543 = ORIENTED_EDGE ( 'NONE', *, *, #9530, .T. ) ;
#12544 = EDGE_CURVE ( 'NONE', #12308, #9734, #16364, .T. ) ;
#12545 = ORIENTED_EDGE ( 'NONE', *, *, #9427, .F. ) ;
#12546 = PRODUCT ( 'Servo-Body', 'Servo-Body', '', ( #17440 ) ) ;
#12547 = ORIENTED_EDGE ( 'NONE', *, *, #7414, .T. ) ;
#12548 =( NAMED_UNIT ( * ) SI_UNIT ( $, .STERADIAN. ) SOLID_ANGLE_UNIT ( ) );
#12549 = CARTESIAN_POINT ( 'NONE',  ( -79.21172376363730905, 140.1316991070070515, 501.4510136243916918 ) ) ;
#12550 = ORIENTED_EDGE ( 'NONE', *, *, #18214, .T. ) ;
#12551 = EDGE_CURVE ( 'NONE', #17102, #2599, #1990, .T. ) ;
#12552 = DIRECTION ( 'NONE',  ( 0.000000000000000000, 0.000000000000000000, 1.000000000000000000 ) ) ;
#12553 = FACE_OUTER_BOUND ( 'NONE', #7301, .T. ) ;
#12554 = EDGE_LOOP ( 'NONE', ( #12836, #5573, #5249, #8019 ) ) ;
#12555 = CIRCLE ( 'NONE', #19763, 4.999999999999997335 ) ;
#12556 = DIRECTION ( 'NONE',  ( -0.000000000000000000, -1.000000000000000000, -0.000000000000000000 ) ) ;
#12557 = AXIS2_PLACEMENT_3D ( 'NONE', #7447, #13915, #10729 ) ;
#12558 = CARTESIAN_POINT ( 'NONE',  ( 53.48937290013659407, 145.9162550801369491, 250.0000000000000000 ) ) ;
#12559 = DIRECTION ( 'NONE',  ( 0.000000000000000000, 0.000000000000000000, 1.000000000000000000 ) ) ;
#12560 = DIRECTION ( 'NONE',  ( 0.000000000000000000, 0.000000000000000000, 1.000000000000000000 ) ) ;
#12561 = DIRECTION ( 'NONE',  ( 0.000000000000000000, 1.000000000000000000, 0.000000000000000000 ) ) ;
#12562 = FACE_OUTER_BOUND ( 'NONE', #30, .T. ) ;
#12563 = DIRECTION ( 'NONE',  ( 1.000000000000000000, 0.000000000000000000, -0.000000000000000000 ) ) ;
#12564 = CARTESIAN_POINT ( 'NONE',  ( 0.000000000000000000, 66.00000000000000000, -5.741599279633704455E-16 ) ) ;
#12565 = DIRECTION ( 'NONE',  ( -0.000000000000000000, -0.000000000000000000, -1.000000000000000000 ) ) ;
#12566 = EDGE_CURVE ( 'NONE', #159, #15834, #17569, .T. ) ;
#12567 = ORIENTED_EDGE ( 'NONE', *, *, #17846, .F. ) ;
#12568 = CIRCLE ( 'NONE', #11579, 1.000000000000000888 ) ;
#12569 = EDGE_LOOP ( 'NONE', ( #18742, #15694, #19906, #342 ) ) ;
#12570 = CARTESIAN_POINT ( 'NONE',  ( -82.18192946989108805, 139.7703989349477354, 489.5655098179820470 ) ) ;
#12571 = AXIS2_PLACEMENT_3D ( 'NONE', #7813, #15664, #12451 ) ;
#12572 = ORIENTED_EDGE ( 'NONE', *, *, #10108, .T. ) ;
#12573 = VERTEX_POINT ( 'NONE', #8206 ) ;
#12574 = EDGE_CURVE ( 'NONE', #8097, #4515, #11327, .T. ) ;
#12575 = EDGE_LOOP ( 'NONE', ( #7856, #16812, #11792, #10149 ) ) ;
#12576 = CARTESIAN_POINT ( 'NONE',  ( 31.81980515339464333, 0.000000000000000000, -31.81980515339463622 ) ) ;
#12577 = LINE ( 'NONE', #12794, #19764 ) ;
#12578 = CYLINDRICAL_SURFACE ( 'NONE', #6129, 18.50000000000000000 ) ;
#12579 = ORIENTED_EDGE ( 'NONE', *, *, #18097, .F. ) ;
#12580 = CARTESIAN_POINT ( 'NONE',  ( 5.687501635565830327, 12.64907335584850046, 0.000000000000000000 ) ) ;
#12581 = DIRECTION ( 'NONE',  ( -0.000000000000000000, -0.000000000000000000, 1.000000000000000000 ) ) ;
#12582 = VECTOR ( 'NONE', #4105, 1000.000000000000000 ) ;
#12583 = MECHANICAL_DESIGN_GEOMETRIC_PRESENTATION_REPRESENTATION (  '', ( #5017 ), #15880 ) ;
#12584 = DIRECTION ( 'NONE',  ( 1.000000000000000000, 0.000000000000000000, -0.000000000000000000 ) ) ;
#12585 = DIRECTION ( 'NONE',  ( 0.000000000000000000, 0.000000000000000000, -1.000000000000000000 ) ) ;
#12586 = CARTESIAN_POINT ( 'NONE',  ( -0.6989004220145259572, 140.0033368016316899, 501.2452398760866004 ) ) ;
#12587 = VECTOR ( 'NONE', #17892, 1000.000000000000000 ) ;
#12588 = ORIENTED_EDGE ( 'NONE', *, *, #15189, .F. ) ;
#12589 = CARTESIAN_POINT ( 'NONE',  ( -82.18192946989275072, 140.4048636633015406, 499.8237260975782306 ) ) ;
#12590 = VECTOR ( 'NONE', #3797, 1000.000000000000000 ) ;
#12591 = VERTEX_POINT ( 'NONE', #19409 ) ;
#12592 = VECTOR ( 'NONE', #9232, 1000.000000000000000 ) ;
#12593 =( GEOMETRIC_REPRESENTATION_CONTEXT ( 3 ) GLOBAL_UNCERTAINTY_ASSIGNED_CONTEXT ( ( #19770 ) ) GLOBAL_UNIT_ASSIGNED_CONTEXT ( ( #19505, #17877, #5424 ) ) REPRESENTATION_CONTEXT ( 'NONE', 'WORKASPACE' ) );
#12594 = EDGE_CURVE ( 'NONE', #16393, #11219, #15633, .T. ) ;
#12595 = DIRECTION ( 'NONE',  ( 0.000000000000000000, 0.000000000000000000, -1.000000000000000000 ) ) ;
#12596 = VERTEX_POINT ( 'NONE', #8308 ) ;
#12597 = DIRECTION ( 'NONE',  ( 1.000000000000000000, 0.000000000000000000, -0.000000000000000000 ) ) ;
#12598 = ORIENTED_EDGE ( 'NONE', *, *, #6284, .F. ) ;
#12599 = DIRECTION ( 'NONE',  ( 0.000000000000000000, 0.000000000000000000, -1.000000000000000000 ) ) ;
#12600 = DIRECTION ( 'NONE',  ( -0.000000000000000000, -0.000000000000000000, 1.000000000000000000 ) ) ;
#12601 = DIRECTION ( 'NONE',  ( 0.000000000000000000, 0.000000000000000000, 1.000000000000000000 ) ) ;
#12602 = AXIS2_PLACEMENT_3D ( 'NONE', #12272, #20091, #20300 ) ;
#12603 = CARTESIAN_POINT ( 'NONE',  ( 0.9274145758904028813, 140.4048636662046476, 500.8237260975781737 ) ) ;
#12604 = DIRECTION ( 'NONE',  ( 0.000000000000000000, 0.000000000000000000, 1.000000000000000000 ) ) ;
#12605 = CARTESIAN_POINT ( 'NONE',  ( 5.044974746830580337, 0.000000000000000000, -14.76997474683059153 ) ) ;
#12606 = DIRECTION ( 'NONE',  ( 1.000000000000000000, 0.000000000000000000, 0.000000000000000000 ) ) ;
#12607 = ORIENTED_EDGE ( 'NONE', *, *, #9468, .T. ) ;
#12608 = DIRECTION ( 'NONE',  ( 1.000000000000000000, 5.889072920838430686E-16, -0.000000000000000000 ) ) ;
#12609 = MECHANICAL_DESIGN_GEOMETRIC_PRESENTATION_REPRESENTATION (  '', ( #18508 ), #2715 ) ;
#12610 = MECHANICAL_DESIGN_GEOMETRIC_PRESENTATION_REPRESENTATION (  '', ( #18845 ), #5048 ) ;
#12611 = SURFACE_STYLE_USAGE ( .BOTH. , #6332 ) ;
#12612 = PRODUCT_CONTEXT ( 'NONE', #13053, 'mechanical' ) ;
#12613 = VERTEX_POINT ( 'NONE', #356 ) ;
#12614 = ORIENTED_EDGE ( 'NONE', *, *, #17421, .T. ) ;
#12615 = DIRECTION ( 'NONE',  ( 1.387778780781446415E-16, -1.000000000000000000, 0.000000000000000000 ) ) ;
#12616 = ORIENTED_EDGE ( 'NONE', *, *, #4339, .F. ) ;
#12617 = EDGE_CURVE ( 'NONE', #9609, #16461, #5089, .T. ) ;
#12618 = VERTEX_POINT ( 'NONE', #14273 ) ;
#12619 = AXIS2_PLACEMENT_3D ( 'NONE', #15892, #18847, #6205 ) ;
#12620 = AXIS2_PLACEMENT_3D ( 'NONE', #1193, #7521, #4320 ) ;
#12621 = ORIENTED_EDGE ( 'NONE', *, *, #9123, .F. ) ;
#12622 = DIRECTION ( 'NONE',  ( 1.000000000000000000, 0.000000000000000000, 0.000000000000000000 ) ) ;
#12623 = ORIENTED_EDGE ( 'NONE', *, *, #13345, .T. ) ;
#12624 = VECTOR ( 'NONE', #15592, 1000.000000000000000 ) ;
#12625 = PLANE ( 'NONE',  #7377 ) ;
#12626 = AXIS2_PLACEMENT_3D ( 'NONE', #2204, #19506, #11714 ) ;
#12627 = SURFACE_STYLE_USAGE ( .BOTH. , #15450 ) ;
#12628 = ORIENTED_EDGE ( 'NONE', *, *, #2571, .F. ) ;
#12629 = LINE ( 'NONE', #4590, #14986 ) ;
#12630 = ADVANCED_FACE ( 'NONE', ( #457 ), #6669, .T. ) ;
#12631 = DIRECTION ( 'NONE',  ( 0.000000000000000000, 0.000000000000000000, -1.000000000000000000 ) ) ;
#12632 =( REPRESENTATION_RELATIONSHIP ('NONE','NONE', #12483, #6180 ) REPRESENTATION_RELATIONSHIP_WITH_TRANSFORMATION ( #8086 )SHAPE_REPRESENTATION_RELATIONSHIP( ) );
#12633 =( LENGTH_UNIT ( ) NAMED_UNIT ( * ) SI_UNIT ( .MILLI., .METRE. ) );
#12634 = FACE_OUTER_BOUND ( 'NONE', #13695, .T. ) ;
#12635 = DIRECTION ( 'NONE',  ( 0.000000000000000000, 0.000000000000000000, 1.000000000000000000 ) ) ;
#12636 =( LENGTH_UNIT ( ) NAMED_UNIT ( * ) SI_UNIT ( .MILLI., .METRE. ) );
#12637 = CIRCLE ( 'NONE', #3751, 8.000000000000007105 ) ;
#12638 =( NAMED_UNIT ( * ) SI_UNIT ( $, .STERADIAN. ) SOLID_ANGLE_UNIT ( ) );
#12639 = VECTOR ( 'NONE', #4738, 1000.000000000000000 ) ;
#12640 = ADVANCED_FACE ( 'NONE', ( #5127 ), #11397, .F. ) ;
#12641 = EDGE_LOOP ( 'NONE', ( #18511, #13258 ) ) ;
#12642 = CARTESIAN_POINT ( 'NONE',  ( 143.0892156028631348, 167.9162550801369491, 245.0000000000000000 ) ) ;
#12643 = CARTESIAN_POINT ( 'NONE',  ( 23.00000000000001066, 68.00000000000000000, -36.99999999999999289 ) ) ;
#12644 = DIRECTION ( 'NONE',  ( 0.000000000000000000, 1.000000000000000000, -0.000000000000000000 ) ) ;
#12645 = CARTESIAN_POINT ( 'NONE',  ( -31.00000000000005684, 0.000000000000000000, -23.00000000000000000 ) ) ;
#12646 = AXIS2_PLACEMENT_3D ( 'NONE', #8698, #13360, #14687 ) ;
#12647 = DIRECTION ( 'NONE',  ( 0.000000000000000000, 0.000000000000000000, 1.000000000000000000 ) ) ;
#12648 = CARTESIAN_POINT ( 'NONE',  ( -0.3790084242192233166, 138.8315893944087804, 489.8888383420726313 ) ) ;
#12649 = ORIENTED_EDGE ( 'NONE', *, *, #14197, .F. ) ;
#12650 = VECTOR ( 'NONE', #14364, 1000.000000000000000 ) ;
#12651 = VECTOR ( 'NONE', #2516, 1000.000000000000000 ) ;
#12652 = EDGE_LOOP ( 'NONE', ( #1462, #14685, #14820, #1555, #11602, #12111 ) ) ;
#12653 = CARTESIAN_POINT ( 'NONE',  ( 0.000000000000000000, 80.91625508013694912, 250.0000000000000000 ) ) ;
#12654 = EDGE_CURVE ( 'NONE', #20073, #13760, #475, .T. ) ;
#12655 =( GEOMETRIC_REPRESENTATION_CONTEXT ( 3 ) GLOBAL_UNCERTAINTY_ASSIGNED_CONTEXT ( ( #18154 ) ) GLOBAL_UNIT_ASSIGNED_CONTEXT ( ( #17747, #13132, #5289 ) ) REPRESENTATION_CONTEXT ( 'NONE', 'WORKASPACE' ) );
#12656 = VECTOR ( 'NONE', #18514, 1000.000000000000000 ) ;
#12657 = EDGE_LOOP ( 'NONE', ( #4635, #6173, #19239, #414, #3488, #550, #18769, #665 ) ) ;
#12658 = CARTESIAN_POINT ( 'NONE',  ( 486.8117674897343363, 214.2156642432025251, 245.0000000000000000 ) ) ;
#12659 = CARTESIAN_POINT ( 'NONE',  ( -79.41690675704376190, 139.9142446525435730, 501.0853735595708258 ) ) ;
#12660 = VECTOR ( 'NONE', #19291, 1000.000000000000000 ) ;
#12661 = VERTEX_POINT ( 'NONE', #19803 ) ;
#12662 = CARTESIAN_POINT ( 'NONE',  ( 31.81980515339464333, 11.00000000000000000, -35.11980515339463693 ) ) ;
#12663 = EDGE_CURVE ( 'NONE', #6575, #716, #16548, .T. ) ;
#12664 = FILL_AREA_STYLE_COLOUR ( '', #18817 ) ;
#12665 = ORIENTED_EDGE ( 'NONE', *, *, #13196, .T. ) ;
#12666 = CARTESIAN_POINT ( 'NONE',  ( -64.99999999999995737, 316.7545334744432353, 495.1946179577816451 ) ) ;
#12667 = COLOUR_RGB ( '', 0.31764706, 0.68627451, 0.89019608) ;
#12668 = FILL_AREA_STYLE_COLOUR ( '', #15661 ) ;
#12669 = CIRCLE ( 'NONE', #11332, 13.95000000000000107 ) ;
#12670 = CARTESIAN_POINT ( 'NONE',  ( -2.844883903241206546, 60.97223153686513086, 9.064373830433188672 ) ) ;
#12671 = ADVANCED_FACE ( 'NONE', ( #8711 ), #15003, .F. ) ;
#12672 = LINE ( 'NONE', #16186, #6859 ) ;
#12673 = EDGE_CURVE ( 'NONE', #16197, #1350, #4071, .T. ) ;
#12674 = CARTESIAN_POINT ( 'NONE',  ( 0.9999999999997842837, 140.4048636633015406, 499.8237260975782306 ) ) ;
#12675 =( GEOMETRIC_REPRESENTATION_CONTEXT ( 3 ) GLOBAL_UNCERTAINTY_ASSIGNED_CONTEXT ( ( #8701 ) ) GLOBAL_UNIT_ASSIGNED_CONTEXT ( ( #6096, #6400, #10818 ) ) REPRESENTATION_CONTEXT ( 'NONE', 'WORKASPACE' ) );
#12676 = AXIS2_PLACEMENT_3D ( 'NONE', #3790, #3890, #10164 ) ;
#12677 = CARTESIAN_POINT ( 'NONE',  ( 475.8334540492694487, 134.2156642432025251, 245.0000000000000000 ) ) ;
#12678 = CIRCLE ( 'NONE', #17616, 14.27500000000000036 ) ;
#12679 = ADVANCED_FACE ( 'NONE', ( #8499 ), #4778, .T. ) ;
#12680 = DIRECTION ( 'NONE',  ( -1.000000000000000000, 0.000000000000000000, 0.000000000000000000 ) ) ;
#12681 = EDGE_CURVE ( 'NONE', #12424, #14021, #11906, .T. ) ;
#12682 = ORIENTED_EDGE ( 'NONE', *, *, #585, .F. ) ;
#12683 = VECTOR ( 'NONE', #860, 1000.000000000000000 ) ;
#12684 = PRESENTATION_LAYER_ASSIGNMENT (  '', '', ( #4124 ) ) ;
#12685 = ORIENTED_EDGE ( 'NONE', *, *, #1894, .F. ) ;
#12686 = UNCERTAINTY_MEASURE_WITH_UNIT (LENGTH_MEASURE( 1.000000000000000082E-05 ), #16546, 'distance_accuracy_value', 'NONE');
#12687 = VECTOR ( 'NONE', #20256, 1000.000000000000000 ) ;
#12688 = CARTESIAN_POINT ( 'NONE',  ( 53.48937290013659407, 127.7247684487574304, 252.0000000000000000 ) ) ;
#12689 = ORIENTED_EDGE ( 'NONE', *, *, #4327, .F. ) ;
#12690 = ORIENTED_EDGE ( 'NONE', *, *, #19508, .T. ) ;
#12691 = ORIENTED_EDGE ( 'NONE', *, *, #14197, .T. ) ;
#12692 = CARTESIAN_POINT ( 'NONE',  ( -40.00000000000000000, 19.00000000000000000, 25.99999999999999645 ) ) ;
#12693 = CIRCLE ( 'NONE', #13669, 4.999999999999997335 ) ;
#12694 = CARTESIAN_POINT ( 'NONE',  ( 109.4893729001365870, 209.7811923590224978, 348.0151256184570343 ) ) ;
#12695 = DIRECTION ( 'NONE',  ( -0.000000000000000000, -0.000000000000000000, 1.000000000000000000 ) ) ;
#12696 =( NAMED_UNIT ( * ) SI_UNIT ( $, .STERADIAN. ) SOLID_ANGLE_UNIT ( ) );
#12697 = AXIS2_PLACEMENT_3D ( 'NONE', #20018, #4087, #10367 ) ;
#12698 = CARTESIAN_POINT ( 'NONE',  ( -32.00000000000000711, 6.000000000000000000, -22.00000000000000355 ) ) ;
#12699 = DIRECTION ( 'NONE',  ( 0.000000000000000000, 0.000000000000000000, 1.000000000000000000 ) ) ;
#12700 = DIRECTION ( 'NONE',  ( 0.000000000000000000, -1.000000000000000000, 0.000000000000000000 ) ) ;
#12701 =( LENGTH_UNIT ( ) NAMED_UNIT ( * ) SI_UNIT ( .MILLI., .METRE. ) );
#12702 = CYLINDRICAL_SURFACE ( 'NONE', #19825, 3.883636366625808911 ) ;
#12703 = AXIS2_PLACEMENT_3D ( 'NONE', #5802, #13821, #16827 ) ;
#12704 = VERTEX_POINT ( 'NONE', #17979 ) ;
#12705 = CARTESIAN_POINT ( 'NONE',  ( 1.224999999999999867, -15.25000000000000000, -1.867586368699713770E-15 ) ) ;
#12706 = ADVANCED_FACE ( 'NONE', ( #15192 ), #16664, .F. ) ;
#12707 = DIRECTION ( 'NONE',  ( 0.000000000000000000, 1.000000000000000000, -0.000000000000000000 ) ) ;
#12708 = VECTOR ( 'NONE', #2262, 1000.000000000000000 ) ;
#12709 = EDGE_CURVE ( 'NONE', #17965, #12453, #7081, .T. ) ;
#12710 = EDGE_CURVE ( 'NONE', #19242, #19318, #9052, .T. ) ;
#12711 = CIRCLE ( 'NONE', #14346, 3.300000000000000711 ) ;
#12712 = VERTEX_POINT ( 'NONE', #11709 ) ;
#12713 = FILL_AREA_STYLE ('',( #9587 ) ) ;
#12714 = VERTEX_POINT ( 'NONE', #8592 ) ;
#12715 = DIRECTION ( 'NONE',  ( -6.263247009234064878E-17, 0.6381222063396385646, -0.7699350945217602327 ) ) ;
#12716 = CARTESIAN_POINT ( 'NONE',  ( 31.81980515339464333, 0.000000000000000000, 31.81980515339463622 ) ) ;
#12717 = EDGE_LOOP ( 'NONE', ( #7004, #6335, #15367, #2255 ) ) ;
#12718 = DIRECTION ( 'NONE',  ( 0.000000000000000000, 0.000000000000000000, 1.000000000000000000 ) ) ;
#12719 = PRESENTATION_STYLE_ASSIGNMENT (( #4664 ) ) ;
#12720 = TOROIDAL_SURFACE ( 'NONE', #9408, 14.27500000000000036, 0.6999999999999999556 ) ;
#12721 = CARTESIAN_POINT ( 'NONE',  ( 21.00000000000000000, 19.00000000000000000, 35.00000000000001421 ) ) ;
#12722 = AXIS2_PLACEMENT_3D ( 'NONE', #3405, #17625, #9684 ) ;
#12723 = CARTESIAN_POINT ( 'NONE',  ( -0.08504567063205197008, 140.3618719181226879, 501.8057946578301198 ) ) ;
#12724 = FACE_OUTER_BOUND ( 'NONE', #12808, .T. ) ;
#12725 = CARTESIAN_POINT ( 'NONE',  ( -22.99999999999999645, 68.00000000000000000, 37.00000000000002132 ) ) ;
#12726 = CARTESIAN_POINT ( 'NONE',  ( -79.99999999999995737, 219.7545334744432921, 512.1946179577817020 ) ) ;
#12727 = VERTEX_POINT ( 'NONE', #943 ) ;
#12728 = CARTESIAN_POINT ( 'NONE',  ( -20.99999999999999645, 19.00000000000000000, -31.00000000000003908 ) ) ;
#12729 = DIRECTION ( 'NONE',  ( -1.000000000000000000, 0.000000000000000000, -1.734723475976807094E-15 ) ) ;
#12730 = ITEM_DEFINED_TRANSFORMATION ( 'NONE', 'NONE', #13937,  #2741 ) ;
#12731 = AXIS2_PLACEMENT_3D ( 'NONE', #2558, #15362, #13596 ) ;
#12732 = PRODUCT_DEFINITION_SHAPE ( 'NONE', 'NONE',  #20373 ) ;
#12733 = EDGE_CURVE ( 'NONE', #1663, #140, #7271, .T. ) ;
#12734 = VERTEX_POINT ( 'NONE', #11806 ) ;
#12735 = ORIENTED_EDGE ( 'NONE', *, *, #16373, .F. ) ;
#12736 = SURFACE_STYLE_FILL_AREA ( #4796 ) ;
#12737 = ORIENTED_EDGE ( 'NONE', *, *, #5893, .F. ) ;
#12738 = ORIENTED_EDGE ( 'NONE', *, *, #9718, .F. ) ;
#12739 = ORIENTED_EDGE ( 'NONE', *, *, #6643, .F. ) ;
#12740 = VECTOR ( 'NONE', #9568, 1000.000000000000000 ) ;
#12741 = DIRECTION ( 'NONE',  ( 0.000000000000000000, 0.000000000000000000, 1.000000000000000000 ) ) ;
#12742 = ORIENTED_EDGE ( 'NONE', *, *, #16318, .F. ) ;
#12743 = SURFACE_SIDE_STYLE ('',( #9324 ) ) ;
#12744 = DIRECTION ( 'NONE',  ( 0.000000000000000000, 1.000000000000000000, 0.000000000000000000 ) ) ;
#12745 = CARTESIAN_POINT ( 'NONE',  ( -81.00000000000127898, 139.7703989349477354, 489.5655098179835818 ) ) ;
#12746 = CARTESIAN_POINT ( 'NONE',  ( 5.569974746830579804, 0.000000000000000000, -14.76997474683060041 ) ) ;
#12747 = CARTESIAN_POINT ( 'NONE',  ( -18.00000000000001421, 10.00000000000000000, 37.00000000000000711 ) ) ;
#12748 = CARTESIAN_POINT ( 'NONE',  ( -26.00000000000002842, 3.000000000000000000, -39.99999999999999289 ) ) ;
#12749 = CARTESIAN_POINT ( 'NONE',  ( 31.00000000000000000, 19.00000000000000000, 30.99999999999999289 ) ) ;
#12750 = CARTESIAN_POINT ( 'NONE',  ( -0.3969782420128915579, 38.01989097161666109, 9.493666329891928157 ) ) ;
#12751 = ORIENTED_EDGE ( 'NONE', *, *, #1919, .F. ) ;
#12752 = FACE_OUTER_BOUND ( 'NONE', #8170, .T. ) ;
#12753 = SURFACE_STYLE_USAGE ( .BOTH. , #17463 ) ;
#12754 = FACE_OUTER_BOUND ( 'NONE', #1054, .T. ) ;
#12755 = DIRECTION ( 'NONE',  ( 1.000000000000000000, 0.000000000000000000, 0.000000000000000000 ) ) ;
#12756 = DIRECTION ( 'NONE',  ( 3.968396791731440098E-12, 0.000000000000000000, -1.000000000000000000 ) ) ;
#12757 = LINE ( 'NONE', #4702, #19487 ) ;
#12758 = CARTESIAN_POINT ( 'NONE',  ( -0.5568521349156368982, 138.8628622585138430, 489.6726277272926495 ) ) ;
#12759 = CARTESIAN_POINT ( 'NONE',  ( 5.569974746830579804, 1.808800229719333629E-15, 14.76997474683060041 ) ) ;
#12760 = LINE ( 'NONE', #4917, #9064 ) ;
#12761 = VECTOR ( 'NONE', #15142, 1000.000000000000000 ) ;
#12762 = PRODUCT_RELATED_PRODUCT_CATEGORY ( 'part', '', ( #9575 ) ) ;
#12763 = EDGE_LOOP ( 'NONE', ( #19796, #5485, #20285, #11817 ) ) ;
#12764 = DIRECTION ( 'NONE',  ( 1.000000000000000000, 0.000000000000000000, 0.000000000000000000 ) ) ;
#12765 = DIRECTION ( 'NONE',  ( 1.000000000000000000, 0.000000000000000000, 0.000000000000000000 ) ) ;
#12766 = EDGE_LOOP ( 'NONE', ( #16079, #6973, #8127, #4850 ) ) ;
#12767 = CARTESIAN_POINT ( 'NONE',  ( 463.8334540492693350, 134.2156642432025251, 250.0000000000000000 ) ) ;
#12768 = DIRECTION ( 'NONE',  ( -0.000000000000000000, -1.000000000000000000, -0.000000000000000000 ) ) ;
#12769 = VERTEX_POINT ( 'NONE', #19611 ) ;
#12770 = EDGE_CURVE ( 'NONE', #19819, #12373, #18065, .T. ) ;
#12771 = CARTESIAN_POINT ( 'NONE',  ( 0.000000000000000000, -3.000000000000000000, -18.50000000000000000 ) ) ;
#12772 = SURFACE_SIDE_STYLE ('',( #3180 ) ) ;
#12773 = DIRECTION ( 'NONE',  ( 0.000000000000000000, 0.7817866094812263578, 0.6235460666509320404 ) ) ;
#12774 = CARTESIAN_POINT ( 'NONE',  ( -211.5106270998635409, 103.1299228374912360, 220.6387154965113382 ) ) ;
#12775 = AXIS2_PLACEMENT_3D ( 'NONE', #4069, #10552, #18278 ) ;
#12776 = DIRECTION ( 'NONE',  ( 1.000000000000000000, -0.000000000000000000, 3.854941057726249930E-16 ) ) ;
#12777 = CARTESIAN_POINT ( 'NONE',  ( 98.48937290013660117, 167.9162550801369491, 250.0000000000000000 ) ) ;
#12778 = PLANE ( 'NONE',  #19161 ) ;
#12779 = CARTESIAN_POINT ( 'NONE',  ( -39.99999999999999289, 11.00000000000000000, 34.99999999999997868 ) ) ;
#12780 = CIRCLE ( 'NONE', #5859, 10.00000000000000888 ) ;
#12781 = DIRECTION ( 'NONE',  ( -1.135258727068399668E-15, 0.000000000000000000, 1.000000000000000000 ) ) ;
#12782 =( NAMED_UNIT ( * ) PLANE_ANGLE_UNIT ( ) SI_UNIT ( $, .RADIAN. ) );
#12783 = EDGE_CURVE ( 'NONE', #10866, #11940, #7865, .T. ) ;
#12784 = ORIENTED_EDGE ( 'NONE', *, *, #14289, .T. ) ;
#12785 = EDGE_LOOP ( 'NONE', ( #9266, #1636 ) ) ;
#12786 = ADVANCED_FACE ( 'NONE', ( #10961 ), #18877, .T. ) ;
#12787 = CARTESIAN_POINT ( 'NONE',  ( 498.8334540492693918, 214.2156642432025251, 0.000000000000000000 ) ) ;
#12788 = EDGE_LOOP ( 'NONE', ( #4846, #8703 ) ) ;
#12789 = ORIENTED_EDGE ( 'NONE', *, *, #13174, .F. ) ;
#12790 = ORIENTED_EDGE ( 'NONE', *, *, #2858, .T. ) ;
#12791 = DIRECTION ( 'NONE',  ( 1.000000000000000000, 0.000000000000000000, 0.000000000000000000 ) ) ;
#12792 = ADVANCED_FACE ( 'NONE', ( #29 ), #18584, .F. ) ;
#12793 = CIRCLE ( 'NONE', #7202, 10.00000000000000888 ) ;
#12794 = CARTESIAN_POINT ( 'NONE',  ( 78.48937290013660117, 145.9162550801369491, -140.0000000000001137 ) ) ;
#12795 = CARTESIAN_POINT ( 'NONE',  ( 2.204364238465236069E-16, 66.00000000000000000, -1.800000000000000711 ) ) ;
#12796 = DIRECTION ( 'NONE',  ( -0.000000000000000000, -0.000000000000000000, -1.000000000000000000 ) ) ;
#12797 = CARTESIAN_POINT ( 'NONE',  ( 0.3969782420128937228, 62.98010902838336023, 9.493666329891928157 ) ) ;
#12798 = PLANE ( 'NONE',  #11099 ) ;
#12799 = EDGE_CURVE ( 'NONE', #3014, #5094, #6021, .T. ) ;
#12800 = DIRECTION ( 'NONE',  ( -0.000000000000000000, 1.000000000000000000, -0.000000000000000000 ) ) ;
#12801 = CARTESIAN_POINT ( 'NONE',  ( 0.000000000000000000, 0.000000000000000000, 0.000000000000000000 ) ) ;
#12802 = ORIENTED_EDGE ( 'NONE', *, *, #3599, .F. ) ;
#12803 = CARTESIAN_POINT ( 'NONE',  ( 31.81980515339464333, 0.000000000000000000, 35.11980515339463693 ) ) ;
#12804 = EDGE_CURVE ( 'NONE', #1294, #4349, #6136, .T. ) ;
#12805 = AXIS2_PLACEMENT_3D ( 'NONE', #17436, #3137, #17138 ) ;
#12806 = ORIENTED_EDGE ( 'NONE', *, *, #16098, .T. ) ;
#12807 = DIRECTION ( 'NONE',  ( 0.000000000000000000, 0.000000000000000000, 1.000000000000000000 ) ) ;
#12808 = EDGE_LOOP ( 'NONE', ( #3554, #14004, #18258, #2950 ) ) ;
#12809 = EDGE_CURVE ( 'NONE', #10759, #2483, #18777, .T. ) ;
#12810 = ORIENTED_EDGE ( 'NONE', *, *, #8535, .T. ) ;
#12811 = LINE ( 'NONE', #19069, #2120 ) ;
#12812 = LINE ( 'NONE', #4976, #6614 ) ;
#12813 = ORIENTED_EDGE ( 'NONE', *, *, #10, .F. ) ;
#12814 = EDGE_CURVE ( 'NONE', #9609, #12110, #14057, .T. ) ;
#12815 = DIRECTION ( 'NONE',  ( 0.000000000000000000, 0.000000000000000000, 1.000000000000000000 ) ) ;
#12816 = CARTESIAN_POINT ( 'NONE',  ( 1.181929469892980755, 139.7545334744432637, 496.6642397995874489 ) ) ;
#12817 = AXIS2_PLACEMENT_3D ( 'NONE', #8883, #15173, #8982 ) ;
#12818 = AXIS2_PLACEMENT_3D ( 'NONE', #12749, #17678, #20345 ) ;
#12819 = CARTESIAN_POINT ( 'NONE',  ( -1.214306433183764966E-14, 141.6406393683235194, 501.8237260975781737 ) ) ;
#12820 = DIRECTION ( 'NONE',  ( 0.000000000000000000, 1.000000000000000000, 0.000000000000000000 ) ) ;
#12821 = DIRECTION ( 'NONE',  ( 6.123031769111888756E-17, -1.000000000000000000, -3.749151804555344967E-33 ) ) ;
#12822 = CARTESIAN_POINT ( 'NONE',  ( 178.4893729001365443, 167.9162550801369491, 250.0000000000000000 ) ) ;
#12823 = DIRECTION ( 'NONE',  ( 0.000000000000000000, 0.000000000000000000, 1.000000000000000000 ) ) ;
#12824 = ORIENTED_EDGE ( 'NONE', *, *, #954, .T. ) ;
#12825 = DIRECTION ( 'NONE',  ( -1.000000000000000000, -0.000000000000000000, -0.000000000000000000 ) ) ;
#12826 = CARTESIAN_POINT ( 'NONE',  ( 22.99999999999997513, 0.000000000000000000, 31.00000000000005684 ) ) ;
#12827 = CARTESIAN_POINT ( 'NONE',  ( -82.18192946989245229, 139.7545334744432637, 491.0690926367355473 ) ) ;
#12828 = PRODUCT_CONTEXT ( 'NONE', #366, 'mechanical' ) ;
#12829 = ORIENTED_EDGE ( 'NONE', *, *, #11343, .T. ) ;
#12830 = DIRECTION ( 'NONE',  ( -0.000000000000000000, 1.000000000000000000, -0.000000000000000000 ) ) ;
#12831 = VERTEX_POINT ( 'NONE', #7665 ) ;
#12832 = VECTOR ( 'NONE', #3077, 1000.000000000000000 ) ;
#12833 = STYLED_ITEM ( 'NONE', ( #1933 ), #6418 ) ;
#12834 = VECTOR ( 'NONE', #2643, 1000.000000000000000 ) ;
#12835 = EDGE_CURVE ( 'NONE', #4170, #19900, #2712, .T. ) ;
#12836 = ORIENTED_EDGE ( 'NONE', *, *, #19459, .T. ) ;
#12837 = DIRECTION ( 'NONE',  ( 0.000000000000000000, 1.000000000000000000, 0.000000000000000000 ) ) ;
#12838 = SURFACE_STYLE_USAGE ( .BOTH. , #5001 ) ;
#12839 = ORIENTED_EDGE ( 'NONE', *, *, #2038, .F. ) ;
#12840 = CARTESIAN_POINT ( 'NONE',  ( 1.347066989204613998E-15, 0.000000000000000000, 22.00000000000000000 ) ) ;
#12841 = SURFACE_STYLE_FILL_AREA ( #15837 ) ;
#12842 = ORIENTED_EDGE ( 'NONE', *, *, #7506, .F. ) ;
#12843 = CARTESIAN_POINT ( 'NONE',  ( -78.99999999999995737, 138.7545334744432637, 510.3921618609452935 ) ) ;
#12844 = LINE ( 'NONE', #3468, #12180 ) ;
#12845 = AXIS2_PLACEMENT_3D ( 'NONE', #12759, #13877, #15657 ) ;
#12846 =( NAMED_UNIT ( * ) SI_UNIT ( $, .STERADIAN. ) SOLID_ANGLE_UNIT ( ) );
#12847 = FACE_OUTER_BOUND ( 'NONE', #14234, .T. ) ;
#12848 = AXIS2_PLACEMENT_3D ( 'NONE', #6380, #7193, #12038 ) ;
#12849 = PRESENTATION_STYLE_ASSIGNMENT (( #9748 ) ) ;
#12850 = CIRCLE ( 'NONE', #4290, 10.00000000000000888 ) ;
#12851 = CARTESIAN_POINT ( 'NONE',  ( -40.00000000000000711, 8.000000000000000000, -26.00000000000000000 ) ) ;
#12852 = ORIENTED_EDGE ( 'NONE', *, *, #10292, .T. ) ;
#12853 = DIRECTION ( 'NONE',  ( -1.000000000000000000, -9.815121534730718631E-17, 0.000000000000000000 ) ) ;
#12854 = FACE_BOUND ( 'NONE', #3485, .T. ) ;
#12855 = CARTESIAN_POINT ( 'NONE',  ( -78.99999999999995737, 216.7545334744432921, 477.3411705753777596 ) ) ;
#12856 = CARTESIAN_POINT ( 'NONE',  ( 468.8334540492694487, 214.2156642432025251, 250.0000000000000000 ) ) ;
#12857 = DIRECTION ( 'NONE',  ( 6.123031769111888756E-17, 0.000000000000000000, 1.000000000000000000 ) ) ;
#12858 = ORIENTED_EDGE ( 'NONE', *, *, #12733, .T. ) ;
#12859 = CARTESIAN_POINT ( 'NONE',  ( 25.99999999999998224, 8.000000000000000000, -32.99999999999999289 ) ) ;
#12860 =( NAMED_UNIT ( * ) SI_UNIT ( $, .STERADIAN. ) SOLID_ANGLE_UNIT ( ) );
#12861 = ORIENTED_EDGE ( 'NONE', *, *, #12770, .F. ) ;
#12862 = ORIENTED_EDGE ( 'NONE', *, *, #9042, .T. ) ;
#12863 = ORIENTED_EDGE ( 'NONE', *, *, #16427, .F. ) ;
#12864 = AXIS2_PLACEMENT_3D ( 'NONE', #13864, #6044, #4498 ) ;
#12865 = AXIS2_PLACEMENT_3D ( 'NONE', #5394, #12821, #5292 ) ;
#12866 = COLOUR_RGB ( '', 0.08235294, 0.09019608, 0.10196078) ;
#12867 = ORIENTED_EDGE ( 'NONE', *, *, #9245, .T. ) ;
#12868 = DIRECTION ( 'NONE',  ( 0.000000000000000000, 1.000000000000000000, 0.000000000000000000 ) ) ;
#12869 = CARTESIAN_POINT ( 'NONE',  ( -79.15851041973368751, 140.2141937887648453, 501.5802637535626900 ) ) ;
#12870 = EDGE_LOOP ( 'NONE', ( #1216, #6653, #20245, #17915, #390, #18265 ) ) ;
#12871 = LINE ( 'NONE', #3176, #11339 ) ;
#12872 = ADVANCED_FACE ( 'NONE', ( #4478 ), #16953, .F. ) ;
#12873 = DIRECTION ( 'NONE',  ( -0.000000000000000000, -1.000000000000000000, -0.000000000000000000 ) ) ;
#12874 = ORIENTED_EDGE ( 'NONE', *, *, #2694, .T. ) ;
#12875 = DIRECTION ( 'NONE',  ( -1.000000000000000000, 0.000000000000000000, -0.000000000000000000 ) ) ;
#12876 = FACE_OUTER_BOUND ( 'NONE', #3136, .T. ) ;
#12877 = PRESENTATION_STYLE_ASSIGNMENT (( #3690 ) ) ;
#12878 = CARTESIAN_POINT ( 'NONE',  ( 5.044974746830580337, 1.808800229719332446E-15, 14.76997474683059153 ) ) ;
#12879 = COLOUR_RGB ( '', 0.09019608, 0.27058824, 0.51372549) ;
#12880 = DIRECTION ( 'NONE',  ( 3.328238341717372086E-14, 0.000000000000000000, -1.000000000000000000 ) ) ;
#12881 = PRESENTATION_LAYER_ASSIGNMENT (  '', '', ( #15509 ) ) ;
#12882 = DIRECTION ( 'NONE',  ( -0.000000000000000000, -1.000000000000000000, -0.000000000000000000 ) ) ;
#12883 = DIRECTION ( 'NONE',  ( 0.000000000000000000, 1.000000000000000000, 0.000000000000000000 ) ) ;
#12884 = DIRECTION ( 'NONE',  ( 0.000000000000000000, 1.000000000000000000, 0.000000000000000000 ) ) ;
#12885 = CARTESIAN_POINT ( 'NONE',  ( 20.99999999999996092, 3.000000000000000000, 35.00000000000000711 ) ) ;
#12886 = ORIENTED_EDGE ( 'NONE', *, *, #10033, .F. ) ;
#12887 = EDGE_CURVE ( 'NONE', #14748, #11627, #15403, .T. ) ;
#12888 = ORIENTED_EDGE ( 'NONE', *, *, #18797, .T. ) ;
#12889 = ORIENTED_EDGE ( 'NONE', *, *, #11816, .F. ) ;
#12890 = UNCERTAINTY_MEASURE_WITH_UNIT (LENGTH_MEASURE( 1.000000000000000082E-05 ), #19405, 'distance_accuracy_value', 'NONE');
#12891 = VERTEX_POINT ( 'NONE', #13843 ) ;
#12892 = ORIENTED_EDGE ( 'NONE', *, *, #13557, .T. ) ;
#12893 = COLOUR_RGB ( '', 0.40784314, 0.44705882, 0.49803922) ;
#12894 = VERTEX_POINT ( 'NONE', #20117 ) ;
#12895 = DIRECTION ( 'NONE',  ( 0.000000000000000000, 0.000000000000000000, 1.000000000000000000 ) ) ;
#12896 = AXIS2_PLACEMENT_3D ( 'NONE', #4533, #13604, #10812 ) ;
#12897 = VECTOR ( 'NONE', #18442, 1000.000000000000000 ) ;
#12898 = LINE ( 'NONE', #7937, #9675 ) ;
#12899 = DIRECTION ( 'NONE',  ( -0.000000000000000000, -0.000000000000000000, 1.000000000000000000 ) ) ;
#12900 = CYLINDRICAL_SURFACE ( 'NONE', #1592, 10.00000000000000888 ) ;
#12901 = FACE_OUTER_BOUND ( 'NONE', #13383, .T. ) ;
#12902 = PRODUCT_DEFINITION_SHAPE ( 'NONE', 'NONE',  #20384 ) ;
#12903 = EDGE_LOOP ( 'NONE', ( #18900, #4997, #1498, #15314 ) ) ;
#12904 = EDGE_CURVE ( 'NONE', #5141, #1964, #9199, .T. ) ;
#12905 = FACE_OUTER_BOUND ( 'NONE', #10399, .T. ) ;
#12906 = DIRECTION ( 'NONE',  ( 0.000000000000000000, 0.000000000000000000, 1.000000000000000000 ) ) ;
#12907 = CARTESIAN_POINT ( 'NONE',  ( -26.00000000000001776, 8.000000000000000000, 33.00000000000000711 ) ) ;
#12908 = CARTESIAN_POINT ( 'NONE',  ( 0.000000000000000000, 5.000000000000000888, -150.0000000000000000 ) ) ;
#12909 = ADVANCED_FACE ( 'NONE', ( #7776 ), #6228, .F. ) ;
#12910 = DIRECTION ( 'NONE',  ( -0.000000000000000000, -1.000000000000000000, -0.000000000000000000 ) ) ;
#12911 = AXIS2_PLACEMENT_3D ( 'NONE', #5428, #6882, #17687 ) ;
#12912 = EDGE_CURVE ( 'NONE', #1482, #8271, #18570, .T. ) ;
#12913 = ORIENTED_EDGE ( 'NONE', *, *, #6504, .T. ) ;
#12914 = ORIENTED_EDGE ( 'NONE', *, *, #18188, .F. ) ;
#12915 = EDGE_CURVE ( 'NONE', #3837, #15261, #9824, .T. ) ;
#12916 = CARTESIAN_POINT ( 'NONE',  ( 503.8334540492693918, 191.8198460455371333, 14.99421986894475012 ) ) ;
#12917 = VERTEX_POINT ( 'NONE', #9725 ) ;
#12918 = CARTESIAN_POINT ( 'NONE',  ( 0.000000000000000000, 26.00000000000000000, 0.000000000000000000 ) ) ;
#12919 = AXIS2_PLACEMENT_3D ( 'NONE', #3551, #9831, #441 ) ;
#12920 = CARTESIAN_POINT ( 'NONE',  ( 40.00000000000001421, -3.000000000000000888, -150.0000000000000000 ) ) ;
#12921 = ORIENTED_EDGE ( 'NONE', *, *, #14532, .F. ) ;
#12922 = DIRECTION ( 'NONE',  ( 0.000000000000000000, -0.000000000000000000, -1.000000000000000000 ) ) ;
#12923 = SURFACE_STYLE_FILL_AREA ( #17648 ) ;
#12925 = ADVANCED_FACE ( 'NONE', ( #3643 ), #9926, .F. ) ;
#12924 = DIRECTION ( 'NONE',  ( 0.000000000000000000, 0.000000000000000000, -1.000000000000000000 ) ) ;
#12926 = VECTOR ( 'NONE', #12978, 1000.000000000000000 ) ;
#12927 = CARTESIAN_POINT ( 'NONE',  ( 21.99999999999998224, 6.000000000000000000, -31.99999999999998579 ) ) ;
#12928 = SURFACE_SIDE_STYLE ('',( #10030 ) ) ;
#12929 = CARTESIAN_POINT ( 'NONE',  ( -211.5106270998635409, 103.1299228374912360, 29.36128450348865471 ) ) ;
#12930 = DIRECTION ( 'NONE',  ( -1.000000000000000000, 0.000000000000000000, -0.000000000000000000 ) ) ;
#12931 = AXIS2_PLACEMENT_3D ( 'NONE', #17067, #2535, #10379 ) ;
#12932 = ORIENTED_EDGE ( 'NONE', *, *, #6342, .T. ) ;
#12933 = CARTESIAN_POINT ( 'NONE',  ( -15.00000000000000000, 317.7545334744432353, 475.1454018718993098 ) ) ;
#12934 = CARTESIAN_POINT ( 'NONE',  ( -36.00000000000000711, 6.000000000000000000, -18.00000000000000355 ) ) ;
#12935 =( NAMED_UNIT ( * ) PLANE_ANGLE_UNIT ( ) SI_UNIT ( $, .RADIAN. ) );
#12936 = EDGE_CURVE ( 'NONE', #19489, #18686, #19888, .T. ) ;
#12937 = VERTEX_POINT ( 'NONE', #19192 ) ;
#12938 = FACE_BOUND ( 'NONE', #482, .T. ) ;
#12939 = ORIENTED_EDGE ( 'NONE', *, *, #5597, .T. ) ;
#12940 = AXIS2_PLACEMENT_3D ( 'NONE', #10581, #16694, #16781 ) ;
#12941 = AXIS2_PLACEMENT_3D ( 'NONE', #3991, #2638, #16583 ) ;
#12942 = EDGE_CURVE ( 'NONE', #19208, #9968, #11028, .T. ) ;
#12943 = VERTEX_POINT ( 'NONE', #5093 ) ;
#12944 = MECHANICAL_DESIGN_GEOMETRIC_PRESENTATION_REPRESENTATION (  '', ( #6686 ), #18832 ) ;
#12945 = ORIENTED_EDGE ( 'NONE', *, *, #4108, .F. ) ;
#12946 = EDGE_CURVE ( 'NONE', #14468, #16599, #14671, .T. ) ;
#12947 = EDGE_LOOP ( 'NONE', ( #19472, #18483 ) ) ;
#12948 = DIRECTION ( 'NONE',  ( 1.000000000000000000, 0.000000000000000000, 0.000000000000000000 ) ) ;
#12949 = DIRECTION ( 'NONE',  ( -0.000000000000000000, -1.000000000000000000, -0.000000000000000000 ) ) ;
#12950 =( LENGTH_UNIT ( ) NAMED_UNIT ( * ) SI_UNIT ( .MILLI., .METRE. ) );
#12951 = AXIS2_PLACEMENT_3D ( 'NONE', #5894, #10940, #18448 ) ;
#12952 = ORIENTED_EDGE ( 'NONE', *, *, #7152, .F. ) ;
#12953 = CARTESIAN_POINT ( 'NONE',  ( -1.273471684549477371E-14, 140.0803823864558808, 488.6808193230643269 ) ) ;
#12954 = ORIENTED_EDGE ( 'NONE', *, *, #3605, .F. ) ;
#12955 = DIRECTION ( 'NONE',  ( -0.000000000000000000, 1.000000000000000000, -0.000000000000000000 ) ) ;
#12956 = CIRCLE ( 'NONE', #13916, 1.000000000000000888 ) ;
#12957 = DIRECTION ( 'NONE',  ( 0.000000000000000000, -1.632680918566406793E-16, 1.000000000000000000 ) ) ;
#12958 = FILL_AREA_STYLE_COLOUR ( '', #9717 ) ;
#12959 = CYLINDRICAL_SURFACE ( 'NONE', #12818, 9.999999999999998224 ) ;
#12960 = CARTESIAN_POINT ( 'NONE',  ( -81.18192946989242387, 138.7545334744432637, 490.5655098179833544 ) ) ;
#12961 = ORIENTED_EDGE ( 'NONE', *, *, #9139, .F. ) ;
#12962 = CARTESIAN_POINT ( 'NONE',  ( 78.48937290013660117, 103.1299228374914065, 220.6387154965113382 ) ) ;
#12963 = PLANE ( 'NONE',  #19162 ) ;
#12964 = CARTESIAN_POINT ( 'NONE',  ( -82.18192946989263703, 147.7545334744432921, 496.6642397995873921 ) ) ;
#12965 = AXIS2_PLACEMENT_3D ( 'NONE', #13011, #11756, #16499 ) ;
#12966 = SURFACE_STYLE_FILL_AREA ( #2110 ) ;
#12967 = EDGE_CURVE ( 'NONE', #1279, #12891, #18912, .T. ) ;
#12968 = ORIENTED_EDGE ( 'NONE', *, *, #9932, .T. ) ;
#12969 = ORIENTED_EDGE ( 'NONE', *, *, #767, .T. ) ;
#12970 = CIRCLE ( 'NONE', #10976, 3.000000000000000000 ) ;
#12971 = CIRCLE ( 'NONE', #765, 15.25000000000000000 ) ;
#12972 = ADVANCED_FACE ( 'NONE', ( #543 ), #16134, .F. ) ;
#12973 = ORIENTED_EDGE ( 'NONE', *, *, #18334, .T. ) ;
#12974 = CARTESIAN_POINT ( 'NONE',  ( 19.99999999999995381, 0.000000000000000000, -36.99999999999999289 ) ) ;
#12975 = VERTEX_POINT ( 'NONE', #6853 ) ;
#12976 = DIRECTION ( 'NONE',  ( 0.000000000000000000, 1.000000000000000000, 0.000000000000000000 ) ) ;
#12977 = COLOUR_RGB ( '', 0.66274510, 0.83137255, 0.94901961) ;
#12978 = DIRECTION ( 'NONE',  ( -0.000000000000000000, -1.000000000000000000, -0.000000000000000000 ) ) ;
#12979 = EDGE_LOOP ( 'NONE', ( #7878, #7951, #12954, #14749 ) ) ;
#12980 = CARTESIAN_POINT ( 'NONE',  ( 143.0892156028631348, 167.9162550801369491, 245.0000000000000000 ) ) ;
#12981 = DIRECTION ( 'NONE',  ( -0.000000000000000000, -1.000000000000000000, -1.632680918566406547E-16 ) ) ;
#12982 = FACE_OUTER_BOUND ( 'NONE', #15452, .T. ) ;
#12983 = FACE_OUTER_BOUND ( 'NONE', #15152, .T. ) ;
#12984 = DIRECTION ( 'NONE',  ( -0.000000000000000000, 1.000000000000000000, -0.000000000000000000 ) ) ;
#12985 = VECTOR ( 'NONE', #14405, 1000.000000000000000 ) ;
#12986 = AXIS2_PLACEMENT_3D ( 'NONE', #9419, #15729, #4990 ) ;
#12987 = LINE ( 'NONE', #190, #8992 ) ;
#12988 = CARTESIAN_POINT ( 'NONE',  ( 0.000000000000000000, 0.000000000000000000, 245.0000000000000000 ) ) ;
#12989 = MECHANICAL_DESIGN_GEOMETRIC_PRESENTATION_REPRESENTATION (  '', ( #5730 ), #13272 ) ;
#12990 = DIRECTION ( 'NONE',  ( 0.000000000000000000, 1.000000000000000000, 0.000000000000000000 ) ) ;
#12991 = AXIS2_PLACEMENT_3D ( 'NONE', #17329, #4963, #20306 ) ;
#12992 = DIRECTION ( 'NONE',  ( 1.000000000000000000, 9.815121534730717399E-17, -0.000000000000000000 ) ) ;
#12993 = CYLINDRICAL_SURFACE ( 'NONE', #2996, 34.00000000000000000 ) ;
#12994 = ORIENTED_EDGE ( 'NONE', *, *, #2975, .T. ) ;
#12995 = VECTOR ( 'NONE', #17531, 1000.000000000000000 ) ;
#12996 = EDGE_CURVE ( 'NONE', #5054, #18073, #3454, .T. ) ;
#12997 = AXIS2_PLACEMENT_3D ( 'NONE', #19551, #15041, #18106 ) ;
#12998 = VERTEX_POINT ( 'NONE', #19388 ) ;
#12999 = AXIS2_PLACEMENT_3D ( 'NONE', #18296, #15110, #19824 ) ;
#13000 = ORIENTED_EDGE ( 'NONE', *, *, #8834, .T. ) ;
#13001 = ORIENTED_EDGE ( 'NONE', *, *, #1540, .T. ) ;
#13002 = AXIS2_PLACEMENT_3D ( 'NONE', #10985, #11089, #14076 ) ;
#13003 = CARTESIAN_POINT ( 'NONE',  ( 25.99999999999996092, 3.000000000000000000, 40.00000000000000711 ) ) ;
#13004 = MECHANICAL_DESIGN_GEOMETRIC_PRESENTATION_REPRESENTATION (  '', ( #13642 ), #18234 ) ;
#13005 = LINE ( 'NONE', #19275, #14293 ) ;
#13006 = AXIS2_PLACEMENT_3D ( 'NONE', #1630, #15796, #1536 ) ;
#13007 = CARTESIAN_POINT ( 'NONE',  ( 10.00000000000000000, 376.0487089519832011, -80.00000000000332534 ) ) ;
#13008 =( LENGTH_UNIT ( ) NAMED_UNIT ( * ) SI_UNIT ( .MILLI., .METRE. ) );
#13009 = CARTESIAN_POINT ( 'NONE',  ( -31.00000000000003197, 0.000000000000000000, -22.99999999999999645 ) ) ;
#13010 = VECTOR ( 'NONE', #11240, 1000.000000000000000 ) ;
#13011 = CARTESIAN_POINT ( 'NONE',  ( 108.9893729001365870, 108.8727366810872468, 338.2196854716659118 ) ) ;
#13012 = CARTESIAN_POINT ( 'NONE',  ( 2.694300560877697759, 61.33377131228787249, 9.110264267939502503 ) ) ;
#13013 = AXIS2_PLACEMENT_3D ( 'NONE', #9355, #4716, #14191 ) ;
#13014 = AXIS2_PLACEMENT_3D ( 'NONE', #17125, #20314, #12597 ) ;
#13015 = SURFACE_STYLE_FILL_AREA ( #17726 ) ;
#13016 = CARTESIAN_POINT ( 'NONE',  ( 458.8334540492693350, 167.8734308960555950, 0.000000000000000000 ) ) ;
#13017 = DIRECTION ( 'NONE',  ( 1.000000000000000000, 0.000000000000000000, 0.000000000000000000 ) ) ;
#13018 = VECTOR ( 'NONE', #12606, 1000.000000000000000 ) ;
#13019 = PRESENTATION_LAYER_ASSIGNMENT (  '', '', ( #1448 ) ) ;
#13020 = CARTESIAN_POINT ( 'NONE',  ( 22.99999999999998224, 0.000000000000000000, 37.00000000000000711 ) ) ;
#13021 =( GEOMETRIC_REPRESENTATION_CONTEXT ( 3 ) GLOBAL_UNCERTAINTY_ASSIGNED_CONTEXT ( ( #3729 ) ) GLOBAL_UNIT_ASSIGNED_CONTEXT ( ( #17342, #14139, #3225 ) ) REPRESENTATION_CONTEXT ( 'NONE', 'WORKASPACE' ) );
#13022 = ORIENTED_EDGE ( 'NONE', *, *, #8620, .T. ) ;
#13023 = VECTOR ( 'NONE', #10281, 1000.000000000000000 ) ;
#13024 = EDGE_CURVE ( 'NONE', #15732, #4060, #9508, .T. ) ;
#13025 = PRESENTATION_LAYER_ASSIGNMENT (  '', '', ( #8414 ) ) ;
#13026 = DIRECTION ( 'NONE',  ( 0.000000000000000000, 0.000000000000000000, -1.000000000000000000 ) ) ;
#13027 = UNCERTAINTY_MEASURE_WITH_UNIT (LENGTH_MEASURE( 1.000000000000000082E-05 ), #4934, 'distance_accuracy_value', 'NONE');
#13028 = VERTEX_POINT ( 'NONE', #1652 ) ;
#13029 =( GEOMETRIC_REPRESENTATION_CONTEXT ( 3 ) GLOBAL_UNCERTAINTY_ASSIGNED_CONTEXT ( ( #5513 ) ) GLOBAL_UNIT_ASSIGNED_CONTEXT ( ( #3497, #17483, #7916 ) ) REPRESENTATION_CONTEXT ( 'NONE', 'WORKASPACE' ) );
#13030 = PRESENTATION_STYLE_ASSIGNMENT (( #19468 ) ) ;
#13031 = ORIENTED_EDGE ( 'NONE', *, *, #18406, .T. ) ;
#13032 = UNCERTAINTY_MEASURE_WITH_UNIT (LENGTH_MEASURE( 1.000000000000000082E-05 ), #3743, 'distance_accuracy_value', 'NONE');
#13033 = DIRECTION ( 'NONE',  ( -0.000000000000000000, -1.000000000000000000, -0.000000000000000000 ) ) ;
#13034 = DIRECTION ( 'NONE',  ( -1.000000000000000000, -0.000000000000000000, -0.000000000000000000 ) ) ;
#13035 = UNCERTAINTY_MEASURE_WITH_UNIT (LENGTH_MEASURE( 1.000000000000000082E-05 ), #11182, 'distance_accuracy_value', 'NONE');
#13036 = VECTOR ( 'NONE', #6053, 1000.000000000000000 ) ;
#13037 = ORIENTED_EDGE ( 'NONE', *, *, #781, .F. ) ;
#13038 = PLANE ( 'NONE',  #10390 ) ;
#13039 = SURFACE_STYLE_FILL_AREA ( #5086 ) ;
#13040 = CARTESIAN_POINT ( 'NONE',  ( 37.00000000000000000, 68.00000000000000000, 23.00000000000001066 ) ) ;
#13041 = ADVANCED_FACE ( 'NONE', ( #9599 ), #15921, .F. ) ;
#13042 = CARTESIAN_POINT ( 'NONE',  ( -38.50085094405407204, 175.4489062796178871, 510.3921618609452935 ) ) ;
#13043 = CARTESIAN_POINT ( 'NONE',  ( -82.18192946989263703, 139.7545334744432637, 496.6642397995874489 ) ) ;
#13044 = CIRCLE ( 'NONE', #14330, 10.00000000000000888 ) ;
#13045 = DIRECTION ( 'NONE',  ( 0.000000000000000000, 0.000000000000000000, -1.000000000000000000 ) ) ;
#13046 = SURFACE_SIDE_STYLE ('',( #5199 ) ) ;
#13047 = EDGE_LOOP ( 'NONE', ( #5886, #3195 ) ) ;
#13048 =( LENGTH_UNIT ( ) NAMED_UNIT ( * ) SI_UNIT ( .MILLI., .METRE. ) );
#13049 = CARTESIAN_POINT ( 'NONE',  ( -26.00000000000000000, 19.00000000000000000, 40.00000000000001421 ) ) ;
#13050 = CARTESIAN_POINT ( 'NONE',  ( -79.99999999999995737, 138.7545334744432637, 510.3921618609452935 ) ) ;
#13051 = VECTOR ( 'NONE', #19926, 1000.000000000000000 ) ;
#13052 = DIRECTION ( 'NONE',  ( -0.000000000000000000, -1.000000000000000000, -0.000000000000000000 ) ) ;
#13053 = APPLICATION_CONTEXT ( 'automotive_design' ) ;
#13054 = EDGE_LOOP ( 'NONE', ( #1200, #1750 ) ) ;
#13055 = ADVANCED_FACE ( 'NONE', ( #4045 ), #11358, .F. ) ;
#13056 = EDGE_CURVE ( 'NONE', #12734, #13149, #922, .T. ) ;
#13057 = ORIENTED_EDGE ( 'NONE', *, *, #435, .F. ) ;
#13058 = VERTEX_POINT ( 'NONE', #7246 ) ;
#13059 = PRESENTATION_LAYER_ASSIGNMENT (  '', '', ( #16023 ) ) ;
#13060 = DIRECTION ( 'NONE',  ( 0.000000000000000000, 0.000000000000000000, -1.000000000000000000 ) ) ;
#13061 = ADVANCED_FACE ( 'NONE', ( #8567 ), #8880, .F. ) ;
#13062 = ORIENTED_EDGE ( 'NONE', *, *, #17411, .T. ) ;
#13063 = UNCERTAINTY_MEASURE_WITH_UNIT (LENGTH_MEASURE( 1.000000000000000082E-05 ), #16258, 'distance_accuracy_value', 'NONE');
#13064 = DIRECTION ( 'NONE',  ( -0.000000000000000000, -1.000000000000000000, -0.000000000000000000 ) ) ;
#13065 = CARTESIAN_POINT ( 'NONE',  ( 2.903217335657448661, 40.21902629923274475, 9.045605051663343943 ) ) ;
#13066 = AXIS2_PLACEMENT_3D ( 'NONE', #9836, #19209, #10426 ) ;
#13067 = ORIENTED_EDGE ( 'NONE', *, *, #11818, .T. ) ;
#13068 = ADVANCED_FACE ( 'NONE', ( #19782 ), #16529, .T. ) ;
#13069 = LINE ( 'NONE', #19404, #18263 ) ;
#13070 = CARTESIAN_POINT ( 'NONE',  ( 25.99999999999996092, 3.000000000000000000, -33.99999999999998579 ) ) ;
#13071 = DIRECTION ( 'NONE',  ( -0.000000000000000000, -1.000000000000000000, -0.000000000000000000 ) ) ;
#13072 = ADVANCED_FACE ( 'NONE', ( #2496 ), #14981, .T. ) ;
#13073 = CARTESIAN_POINT ( 'NONE',  ( -15.00000000000000000, 317.7545334744432353, 475.1454018718993098 ) ) ;
#13074 = CARTESIAN_POINT ( 'NONE',  ( 423.8334540492694487, 191.8198460455371333, 225.0057801310552463 ) ) ;
#13075 = CARTESIAN_POINT ( 'NONE',  ( 1.163414460601643398E-15, 38.00000000000000711, 9.500000000000000000 ) ) ;
#13076 = ORIENTED_EDGE ( 'NONE', *, *, #7506, .T. ) ;
#13077 = CARTESIAN_POINT ( 'NONE',  ( -79.99999999999995737, 147.7545334744432921, 496.6642397995874489 ) ) ;
#13078 = ADVANCED_FACE ( 'NONE', ( #634 ), #13344, .F. ) ;
#13079 = CARTESIAN_POINT ( 'NONE',  ( 111.4893729001366012, 208.2227610943810134, 346.7612763259490407 ) ) ;
#13080 =( NAMED_UNIT ( * ) PLANE_ANGLE_UNIT ( ) SI_UNIT ( $, .RADIAN. ) );
#13081 = ORIENTED_EDGE ( 'NONE', *, *, #9585, .F. ) ;
#13082 = DIRECTION ( 'NONE',  ( 0.000000000000000000, 1.000000000000000000, 0.000000000000000000 ) ) ;
#13083 = LINE ( 'NONE', #10411, #12510 ) ;
#13084 = ADVANCED_BREP_SHAPE_REPRESENTATION ( '', ( #8197, #2741 ), #4080 ) ;
#13085 = VERTEX_POINT ( 'NONE', #17956 ) ;
#13086 = CIRCLE ( 'NONE', #17331, 13.29999999999999893 ) ;
#13087 = EDGE_CURVE ( 'NONE', #2627, #19923, #11572, .T. ) ;
#13088 = ORIENTED_EDGE ( 'NONE', *, *, #18707, .T. ) ;
#13089 = ORIENTED_EDGE ( 'NONE', *, *, #16949, .F. ) ;
#13090 = DIRECTION ( 'NONE',  ( 0.000000000000000000, 0.7071067811865336949, -0.7071067811865614505 ) ) ;
#13091 = EDGE_LOOP ( 'NONE', ( #8144, #11083, #6318, #5601 ) ) ;
#13092 = SURFACE_STYLE_FILL_AREA ( #3273 ) ;
#13093 = ORIENTED_EDGE ( 'NONE', *, *, #8227, .F. ) ;
#13094 = EDGE_CURVE ( 'NONE', #9635, #8551, #8734, .T. ) ;
#13095 = LINE ( 'NONE', #17600, #9206 ) ;
#13096 = DIRECTION ( 'NONE',  ( -1.000000000000000000, 0.000000000000000000, -0.000000000000000000 ) ) ;
#13097 = CARTESIAN_POINT ( 'NONE',  ( -75.00000000000000000, 368.2663108437010919, -87.78239810828596035 ) ) ;
#13098 = SURFACE_SIDE_STYLE ('',( #4932 ) ) ;
#13099 = DIRECTION ( 'NONE',  ( 0.000000000000000000, 0.000000000000000000, -1.000000000000000000 ) ) ;
#13100 = EDGE_CURVE ( 'NONE', #20017, #11746, #13440, .T. ) ;
#13101 =( NAMED_UNIT ( * ) PLANE_ANGLE_UNIT ( ) SI_UNIT ( $, .RADIAN. ) );
#13102 = DIRECTION ( 'NONE',  ( 0.000000000000000000, 0.000000000000000000, -1.000000000000000000 ) ) ;
#13103 = CARTESIAN_POINT ( 'NONE',  ( 31.81980515339464333, 0.000000000000000000, -31.81980515339463622 ) ) ;
#13104 = SURFACE_STYLE_USAGE ( .BOTH. , #14620 ) ;
#13105 = VERTEX_POINT ( 'NONE', #16343 ) ;
#13106 = VECTOR ( 'NONE', #307, 1000.000000000000000 ) ;
#13107 = VERTEX_POINT ( 'NONE', #5585 ) ;
#13108 = ORIENTED_EDGE ( 'NONE', *, *, #4688, .T. ) ;
#13109 = ORIENTED_EDGE ( 'NONE', *, *, #1969, .F. ) ;
#13110 = VERTEX_POINT ( 'NONE', #2180 ) ;
#13111 = CARTESIAN_POINT ( 'NONE',  ( 0.000000000000000000, 66.00000000000000000, 0.000000000000000000 ) ) ;
#13112 = CARTESIAN_POINT ( 'NONE',  ( -22.99999999999999645, 0.000000000000000000, 31.00000000000003908 ) ) ;
#13113 = FACE_OUTER_BOUND ( 'NONE', #9964, .T. ) ;
#13114 =( NAMED_UNIT ( * ) SI_UNIT ( $, .STERADIAN. ) SOLID_ANGLE_UNIT ( ) );
#13115 = FACE_OUTER_BOUND ( 'NONE', #9606, .T. ) ;
#13116 = DIRECTION ( 'NONE',  ( -0.000000000000000000, -1.000000000000000000, 0.000000000000000000 ) ) ;
#13117 = CARTESIAN_POINT ( 'NONE',  ( 2.979937318121946177, 60.39873976293512214, 9.020623939867238761 ) ) ;
#13118 = AXIS2_PLACEMENT_3D ( 'NONE', #14528, #14641, #6508 ) ;
#13119 = DIRECTION ( 'NONE',  ( 0.000000000000000000, 0.000000000000000000, -1.000000000000000000 ) ) ;
#13120 = DIRECTION ( 'NONE',  ( -1.000000000000000000, -6.123031769111888756E-17, 6.123031769111888756E-17 ) ) ;
#13121 = DIRECTION ( 'NONE',  ( -0.000000000000000000, -1.000000000000000000, -0.000000000000000000 ) ) ;
#13122 = DIRECTION ( 'NONE',  ( 7.714098457234357737E-14, 0.000000000000000000, 1.000000000000000000 ) ) ;
#13123 = LINE ( 'NONE', #2159, #12332 ) ;
#13124 = ORIENTED_EDGE ( 'NONE', *, *, #7030, .T. ) ;
#13125 = CIRCLE ( 'NONE', #2881, 35.00000000000000711 ) ;
#13126 = ORIENTED_EDGE ( 'NONE', *, *, #14923, .T. ) ;
#13127 = CARTESIAN_POINT ( 'NONE',  ( 31.00000000000006395, 0.000000000000000000, -22.99999999999999289 ) ) ;
#13128 = ORIENTED_EDGE ( 'NONE', *, *, #13658, .T. ) ;
#13129 = DIRECTION ( 'NONE',  ( 1.000000000000000000, 0.000000000000000000, 0.000000000000000000 ) ) ;
#13130 = DIRECTION ( 'NONE',  ( 0.000000000000000000, 0.000000000000000000, -1.000000000000000000 ) ) ;
#13131 = ORIENTED_EDGE ( 'NONE', *, *, #691, .F. ) ;
#13132 =( NAMED_UNIT ( * ) PLANE_ANGLE_UNIT ( ) SI_UNIT ( $, .RADIAN. ) );
#13133 = EDGE_CURVE ( 'NONE', #3979, #9984, #8481, .T. ) ;
#13134 = DIRECTION ( 'NONE',  ( 0.000000000000000000, 0.000000000000000000, 1.000000000000000000 ) ) ;
#13135 = DIRECTION ( 'NONE',  ( 0.000000000000000000, 0.000000000000000000, -1.000000000000000000 ) ) ;
#13136 = DIRECTION ( 'NONE',  ( -0.8502651466878615727, 0.5263546146162958461, 0.000000000000000000 ) ) ;
#13137 = DIRECTION ( 'NONE',  ( 0.000000000000000000, 0.000000000000000000, 1.000000000000000000 ) ) ;
#13138 = DIRECTION ( 'NONE',  ( 0.000000000000000000, 0.000000000000000000, 1.000000000000000000 ) ) ;
#13139 = ORIENTED_EDGE ( 'NONE', *, *, #9260, .F. ) ;
#13140 = PLANE ( 'NONE',  #4568 ) ;
#13141 = LINE ( 'NONE', #16532, #17905 ) ;
#13142 = CARTESIAN_POINT ( 'NONE',  ( 36.99999999999999289, 10.00000000000000000, 17.99999999999998934 ) ) ;
#13143 = ORIENTED_EDGE ( 'NONE', *, *, #12400, .F. ) ;
#13144 = ORIENTED_EDGE ( 'NONE', *, *, #1024, .T. ) ;
#13145 = EDGE_CURVE ( 'NONE', #6497, #12403, #16430, .T. ) ;
#13146 = ORIENTED_EDGE ( 'NONE', *, *, #13879, .T. ) ;
#13147 = CARTESIAN_POINT ( 'NONE',  ( -32.00000000000000711, 10.00000000000000000, -23.00000000000000000 ) ) ;
#13148 = AXIS2_PLACEMENT_3D ( 'NONE', #16531, #11786, #17754 ) ;
#13149 = VERTEX_POINT ( 'NONE', #15681 ) ;
#13150 = PLANE ( 'NONE',  #19852 ) ;
#13151 = CARTESIAN_POINT ( 'NONE',  ( 1.845421771225094210, 38.60300962669240477, 9.323305159997634206 ) ) ;
#13152 = ORIENTED_EDGE ( 'NONE', *, *, #5992, .T. ) ;
#13153 = SURFACE_STYLE_USAGE ( .BOTH. , #6776 ) ;
#13154 = DIRECTION ( 'NONE',  ( -1.000000000000000000, 0.000000000000000000, 0.000000000000000000 ) ) ;
#13155 = DIRECTION ( 'NONE',  ( -1.000000000000000000, 0.000000000000000000, 0.000000000000000000 ) ) ;
#13156 = EDGE_CURVE ( 'NONE', #7981, #323, #13924, .T. ) ;
#13157 = CARTESIAN_POINT ( 'NONE',  ( -0.7824566857511718876, 38.09717326031902473, 9.469691317190788382 ) ) ;
#13158 = EDGE_LOOP ( 'NONE', ( #13781, #4052, #16073, #824 ) ) ;
#13159 = PLANE ( 'NONE',  #15770 ) ;
#13160 = SURFACE_STYLE_USAGE ( .BOTH. , #19320 ) ;
#13161 = LINE ( 'NONE', #5321, #18167 ) ;
#13162 =( GEOMETRIC_REPRESENTATION_CONTEXT ( 3 ) GLOBAL_UNCERTAINTY_ASSIGNED_CONTEXT ( ( #14849 ) ) GLOBAL_UNIT_ASSIGNED_CONTEXT ( ( #1512, #12782, #14105 ) ) REPRESENTATION_CONTEXT ( 'NONE', 'WORKASPACE' ) );
#13163 = DIRECTION ( 'NONE',  ( 1.000000000000000000, 0.000000000000000000, 0.000000000000000000 ) ) ;
#13164 = AXIS2_PLACEMENT_3D ( 'NONE', #1314, #20305, #19138 ) ;
#13165 = VERTEX_POINT ( 'NONE', #15993 ) ;
#13166 = EDGE_CURVE ( 'NONE', #6182, #12416, #9559, .T. ) ;
#13167 = FACE_OUTER_BOUND ( 'NONE', #12231, .T. ) ;
#13168 = AXIS2_PLACEMENT_3D ( 'NONE', #1360, #18705, #2840 ) ;
#13169 = VERTEX_POINT ( 'NONE', #15876 ) ;
#13170 = VERTEX_POINT ( 'NONE', #11020 ) ;
#13171 = EDGE_CURVE ( 'NONE', #11471, #17234, #5806, .T. ) ;
#13172 = ORIENTED_EDGE ( 'NONE', *, *, #4583, .T. ) ;
#13173 = CARTESIAN_POINT ( 'NONE',  ( 0.000000000000000000, 19.00100000000000122, -18.50000000000000000 ) ) ;
#13174 = EDGE_CURVE ( 'NONE', #14376, #12975, #8634, .T. ) ;
#13175 = DIRECTION ( 'NONE',  ( 0.000000000000000000, 0.000000000000000000, -1.000000000000000000 ) ) ;
#13176 = VECTOR ( 'NONE', #3999, 1000.000000000000000 ) ;
#13177 = ORIENTED_EDGE ( 'NONE', *, *, #18561, .F. ) ;
#13178 = AXIS2_PLACEMENT_3D ( 'NONE', #73, #16183, #184 ) ;
#13179 = DIRECTION ( 'NONE',  ( 0.000000000000000000, -1.000000000000000000, 0.000000000000000000 ) ) ;
#13180 = VECTOR ( 'NONE', #16056, 1000.000000000000000 ) ;
#13181 = FILL_AREA_STYLE ('',( #6894 ) ) ;
#13182 = DIRECTION ( 'NONE',  ( 0.000000000000000000, 0.000000000000000000, 1.000000000000000000 ) ) ;
#13183 = LINE ( 'NONE', #16284, #11934 ) ;
#13184 = SURFACE_STYLE_FILL_AREA ( #10080 ) ;
#13185 = EDGE_CURVE ( 'NONE', #2425, #951, #7648, .T. ) ;
#13186 = CYLINDRICAL_SURFACE ( 'NONE', #12293, 1.000000000000000888 ) ;
#13187 = DIRECTION ( 'NONE',  ( 1.000000000000000000, 0.000000000000000000, 0.000000000000000000 ) ) ;
#13188 = SHAPE_REPRESENTATION_RELATIONSHIP ( 'NONE' , 'NONE' ,  #16597, #14042 ) ;
#13189 = SURFACE_STYLE_FILL_AREA ( #16188 ) ;
#13190 = FACE_OUTER_BOUND ( 'NONE', #12657, .T. ) ;
#13191 = PLANE ( 'NONE',  #16788 ) ;
#13192 = DIRECTION ( 'NONE',  ( -0.000000000000000000, 1.000000000000000000, -0.000000000000000000 ) ) ;
#13193 = DIRECTION ( 'NONE',  ( -0.000000000000000000, -0.000000000000000000, -1.000000000000000000 ) ) ;
#13194 = ORIENTED_EDGE ( 'NONE', *, *, #4218, .F. ) ;
#13195 = CIRCLE ( 'NONE', #4287, 18.50000000000000000 ) ;
#13196 = EDGE_CURVE ( 'NONE', #15883, #10771, #19894, .T. ) ;
#13197 = VECTOR ( 'NONE', #3352, 1000.000000000000000 ) ;
#13198 = MECHANICAL_DESIGN_GEOMETRIC_PRESENTATION_REPRESENTATION (  '', ( #13818 ), #7570 ) ;
#13199 = ORIENTED_EDGE ( 'NONE', *, *, #16983, .F. ) ;
#13200 = ORIENTED_EDGE ( 'NONE', *, *, #4552, .T. ) ;
#13201 = EDGE_LOOP ( 'NONE', ( #11692, #12108, #11578, #11656 ) ) ;
#13202 = ORIENTED_EDGE ( 'NONE', *, *, #19234, .T. ) ;
#13203 = FACE_OUTER_BOUND ( 'NONE', #5916, .T. ) ;
#13204 = CARTESIAN_POINT ( 'NONE',  ( 10.00000000000000000, 301.0487089519832011, -80.00000000000387956 ) ) ;
#13205 = DIRECTION ( 'NONE',  ( 0.000000000000000000, 0.000000000000000000, -1.000000000000000000 ) ) ;
#13206 = CARTESIAN_POINT ( 'NONE',  ( -31.00000000000000000, 19.00000000000000000, -31.00000000000000000 ) ) ;
#13207 = CARTESIAN_POINT ( 'NONE',  ( 111.4893729001366012, 209.4935875941501422, 345.2279431939882670 ) ) ;
#13208 =( GEOMETRIC_REPRESENTATION_CONTEXT ( 3 ) GLOBAL_UNCERTAINTY_ASSIGNED_CONTEXT ( ( #9085 ) ) GLOBAL_UNIT_ASSIGNED_CONTEXT ( ( #5198, #11370, #3642 ) ) REPRESENTATION_CONTEXT ( 'NONE', 'WORKASPACE' ) );
#13209 = LINE ( 'NONE', #10104, #9649 ) ;
#13210 = CARTESIAN_POINT ( 'NONE',  ( 149.0892156028631348, 80.91625508013694912, 245.0000000000000000 ) ) ;
#13211 = CARTESIAN_POINT ( 'NONE',  ( -37.00000000000000711, 0.000000000000000000, 23.00000000000000000 ) ) ;
#13212 = AXIS2_PLACEMENT_3D ( 'NONE', #17929, #3621, #10001 ) ;
#13213 = EDGE_CURVE ( 'NONE', #11163, #17086, #8979, .T. ) ;
#13214 = DIRECTION ( 'NONE',  ( 7.897989220727750531E-17, -0.8046756418431283420, 0.5937146717273790175 ) ) ;
#13215 = CARTESIAN_POINT ( 'NONE',  ( 0.6999999999999999556, -18.50000000000000000, -2.265596578422603396E-15 ) ) ;
#13216 = EDGE_CURVE ( 'NONE', #3885, #14143, #17506, .T. ) ;
#13217 = AXIS2_PLACEMENT_3D ( 'NONE', #18427, #10603, #4234 ) ;
#13218 = AXIS2_PLACEMENT_3D ( 'NONE', #7938, #1523, #11039 ) ;
#13219 = ORIENTED_EDGE ( 'NONE', *, *, #16578, .F. ) ;
#13220 = UNCERTAINTY_MEASURE_WITH_UNIT (LENGTH_MEASURE( 1.000000000000000082E-05 ), #5455, 'distance_accuracy_value', 'NONE');
#13221 = ORIENTED_EDGE ( 'NONE', *, *, #11790, .T. ) ;
#13222 = ORIENTED_EDGE ( 'NONE', *, *, #10607, .T. ) ;
#13223 = EDGE_LOOP ( 'NONE', ( #17177, #12961, #3810, #14930 ) ) ;
#13224 = UNCERTAINTY_MEASURE_WITH_UNIT (LENGTH_MEASURE( 1.000000000000000082E-05 ), #19279, 'distance_accuracy_value', 'NONE');
#13225 = CARTESIAN_POINT ( 'NONE',  ( 463.8334540492693350, 214.2156642432025251, 0.000000000000000000 ) ) ;
#13226 = ORIENTED_EDGE ( 'NONE', *, *, #15906, .T. ) ;
#13227 = CARTESIAN_POINT ( 'NONE',  ( -78.99999999999995737, 152.4824555358011082, 478.3411705753777596 ) ) ;
#13228 = DIRECTION ( 'NONE',  ( 0.000000000000000000, 0.000000000000000000, -1.000000000000000000 ) ) ;
#13229 = MECHANICAL_DESIGN_GEOMETRIC_PRESENTATION_REPRESENTATION (  '', ( #7956 ), #14535 ) ;
#13230 =( NAMED_UNIT ( * ) SI_UNIT ( $, .STERADIAN. ) SOLID_ANGLE_UNIT ( ) );
#13231 = DIRECTION ( 'NONE',  ( 0.000000000000000000, 0.000000000000000000, 1.000000000000000000 ) ) ;
#13232 = LINE ( 'NONE', #8388, #17785 ) ;
#13233 = PRESENTATION_LAYER_ASSIGNMENT (  '', '', ( #19783 ) ) ;
#13234 = ORIENTED_EDGE ( 'NONE', *, *, #11357, .T. ) ;
#13235 = CARTESIAN_POINT ( 'NONE',  ( 1.050000000000000044, 17.52499999999999858, 0.000000000000000000 ) ) ;
#13236 = PLANE ( 'NONE',  #13946 ) ;
#13237 = EDGE_CURVE ( 'NONE', #5387, #5210, #1124, .T. ) ;
#13238 = ORIENTED_EDGE ( 'NONE', *, *, #10255, .F. ) ;
#13239 = EDGE_LOOP ( 'NONE', ( #8436, #17853 ) ) ;
#13240 = COLOUR_RGB ( '', 0.40784314, 0.44705882, 0.49803922) ;
#13241 = DIRECTION ( 'NONE',  ( -0.000000000000000000, -1.000000000000000000, -0.000000000000000000 ) ) ;
#13242 = ORIENTED_EDGE ( 'NONE', *, *, #4226, .F. ) ;
#13243 = CARTESIAN_POINT ( 'NONE',  ( 1.163414460601643398E-15, 38.00000000000000711, 9.500000000000000000 ) ) ;
#13244 = EDGE_LOOP ( 'NONE', ( #11275, #7090, #10969, #9357 ) ) ;
#13245 = DIRECTION ( 'NONE',  ( 0.000000000000000000, 0.000000000000000000, 1.000000000000000000 ) ) ;
#13246 = SURFACE_STYLE_FILL_AREA ( #17869 ) ;
#13247 = VECTOR ( 'NONE', #5240, 1000.000000000000000 ) ;
#13248 = LINE ( 'NONE', #750, #16322 ) ;
#13249 = SURFACE_SIDE_STYLE ('',( #16260 ) ) ;
#13250 = DIRECTION ( 'NONE',  ( 0.000000000000000000, 0.000000000000000000, 1.000000000000000000 ) ) ;
#13251 = EDGE_LOOP ( 'NONE', ( #15059, #1078, #2826, #19337 ) ) ;
#13252 = CARTESIAN_POINT ( 'NONE',  ( -64.99999999999995737, 317.7545334744432353, 475.1454018718993098 ) ) ;
#13253 = DIRECTION ( 'NONE',  ( 1.000000000000000000, -0.000000000000000000, 0.000000000000000000 ) ) ;
#13254 = CARTESIAN_POINT ( 'NONE',  ( 30.99999999999999645, 3.000000000000000000, -25.99999999999999645 ) ) ;
#13255 = CARTESIAN_POINT ( 'NONE',  ( 10.00000000000000000, 306.0487089519837696, -155.0000000000038369 ) ) ;
#13256 = CARTESIAN_POINT ( 'NONE',  ( 182.8664063413478118, 36.11883647564081201, 24.42758688528229527 ) ) ;
#13257 = EDGE_CURVE ( 'NONE', #12618, #1696, #14312, .T. ) ;
#13258 = ORIENTED_EDGE ( 'NONE', *, *, #9804, .T. ) ;
#13259 = PRESENTATION_STYLE_ASSIGNMENT (( #14789 ) ) ;
#13260 = AXIS2_PLACEMENT_3D ( 'NONE', #15642, #12322, #1674 ) ;
#13261 = ORIENTED_EDGE ( 'NONE', *, *, #9880, .F. ) ;
#13262 = MECHANICAL_DESIGN_GEOMETRIC_PRESENTATION_REPRESENTATION (  '', ( #7982 ), #16505 ) ;
#13263 = ORIENTED_EDGE ( 'NONE', *, *, #14666, .T. ) ;
#13264 = ADVANCED_FACE ( 'NONE', ( #18827 ), #12778, .F. ) ;
#13265 = EDGE_LOOP ( 'NONE', ( #2181, #1052 ) ) ;
#13266 = ORIENTED_EDGE ( 'NONE', *, *, #13879, .F. ) ;
#13267 = CARTESIAN_POINT ( 'NONE',  ( 53.48937290013658696, 122.8810204491430369, 322.0399576098686225 ) ) ;
#13268 = VECTOR ( 'NONE', #2789, 1000.000000000000000 ) ;
#13269 = DIRECTION ( 'NONE',  ( 0.000000000000000000, -1.000000000000000000, 0.000000000000000000 ) ) ;
#13270 = CIRCLE ( 'NONE', #17197, 3.300000000000025135 ) ;
#13271 = ORIENTED_EDGE ( 'NONE', *, *, #308, .T. ) ;
#13272 =( GEOMETRIC_REPRESENTATION_CONTEXT ( 3 ) GLOBAL_UNCERTAINTY_ASSIGNED_CONTEXT ( ( #5812 ) ) GLOBAL_UNIT_ASSIGNED_CONTEXT ( ( #4128, #3177, #14299 ) ) REPRESENTATION_CONTEXT ( 'NONE', 'WORKASPACE' ) );
#13273 = CARTESIAN_POINT ( 'NONE',  ( 37.00000000000003553, 3.000000000000000000, 23.00000000000000355 ) ) ;
#13274 = DIRECTION ( 'NONE',  ( 0.000000000000000000, 1.000000000000000000, -0.000000000000000000 ) ) ;
#13275 = PRODUCT_DEFINITION ( 'UNKNOWN', '', #16561, #3702 ) ;
#13276 = TOROIDAL_SURFACE ( 'NONE', #4373, 8.000000000000000000, 1.000000000000000000 ) ;
#13277 = CARTESIAN_POINT ( 'NONE',  ( -26.00000000000001776, 10.00000000000000000, 31.00000000000003553 ) ) ;
#13278 = CARTESIAN_POINT ( 'NONE',  ( 0.000000000000000000, -3.000000000000000000, 0.000000000000000000 ) ) ;
#13279 = SHAPE_REPRESENTATION ( 'HG-KN73JK', ( #4024, #13937, #6727, #17551, #20179, #6678, #15226, #8363 ), #18213 ) ;
#13280 = DIRECTION ( 'NONE',  ( 1.000000000000000000, 0.000000000000000000, 0.000000000000000000 ) ) ;
#13281 = FILL_AREA_STYLE ('',( #8442 ) ) ;
#13282 = AXIS2_PLACEMENT_3D ( 'NONE', #7125, #19157, #5265 ) ;
#13283 = LINE ( 'NONE', #11734, #19652 ) ;
#13284 = EDGE_CURVE ( 'NONE', #6649, #3049, #4935, .T. ) ;
#13285 = SURFACE_STYLE_USAGE ( .BOTH. , #3598 ) ;
#13286 = CARTESIAN_POINT ( 'NONE',  ( -36.99999999999997868, 3.000000000000000000, -19.99999999999999289 ) ) ;
#13287 = CARTESIAN_POINT ( 'NONE',  ( -31.00000000000003197, 0.000000000000000000, -30.99999999999999289 ) ) ;
#13288 = ORIENTED_EDGE ( 'NONE', *, *, #12512, .F. ) ;
#13289 = UNCERTAINTY_MEASURE_WITH_UNIT (LENGTH_MEASURE( 1.000000000000000082E-05 ), #10789, 'distance_accuracy_value', 'NONE');
#13290 = LINE ( 'NONE', #789, #9569 ) ;
#13291 = DIRECTION ( 'NONE',  ( 0.000000000000000000, 1.000000000000000000, 0.000000000000000000 ) ) ;
#13292 = EDGE_CURVE ( 'NONE', #1728, #3836, #4690, .T. ) ;
#13293 = COLOUR_RGB ( '', 0.72549020, 0.75294118, 0.79215686) ;
#13294 = VERTEX_POINT ( 'NONE', #9669 ) ;
#13295 = VECTOR ( 'NONE', #17415, 1000.000000000000000 ) ;
#13296 = ORIENTED_EDGE ( 'NONE', *, *, #7208, .F. ) ;
#13297 = EDGE_CURVE ( 'NONE', #8551, #5165, #2697, .T. ) ;
#13298 = CLOSED_SHELL ( 'NONE', ( #19856, #17398, #8611, #16082, #6418, #8670, #6042, #827, #13886, #8244, #19583, #219, #7987, #7851, #10842, #1960, #6530, #9261, #12216, #11802, #16097, #18833, #11879, #1151, #15140, #11043 ) ) ;
#13299 = VERTEX_POINT ( 'NONE', #12089 ) ;
#13300 = ORIENTED_EDGE ( 'NONE', *, *, #14158, .F. ) ;
#13301 = DIRECTION ( 'NONE',  ( -1.000000000000000000, -0.000000000000000000, -0.000000000000000000 ) ) ;
#13302 = PLANE ( 'NONE',  #8374 ) ;
#13303 = CARTESIAN_POINT ( 'NONE',  ( 0.000000000000000000, -5.000000000000000888, -150.0000000000000000 ) ) ;
#13304 = DIRECTION ( 'NONE',  ( -1.000000000000000000, 0.000000000000000000, 3.854941057726251409E-16 ) ) ;
#13305 = ADVANCED_FACE ( 'NONE', ( #4252 ), #10532, .T. ) ;
#13306 = AXIS2_PLACEMENT_3D ( 'NONE', #3258, #164, #14081 ) ;
#13307 =( NAMED_UNIT ( * ) PLANE_ANGLE_UNIT ( ) SI_UNIT ( $, .RADIAN. ) );
#13308 = VECTOR ( 'NONE', #12141, 1000.000000000000000 ) ;
#13309 = ADVANCED_FACE ( 'NONE', ( #6190, #3074 ), #12464, .T. ) ;
#13310 = SURFACE_SIDE_STYLE ('',( #14833 ) ) ;
#13311 = LINE ( 'NONE', #12214, #16271 ) ;
#13312 = CARTESIAN_POINT ( 'NONE',  ( -25.99999999999999645, 68.00000000000000000, 40.00000000000002132 ) ) ;
#13313 = CARTESIAN_POINT ( 'NONE',  ( -79.24209493944616156, 138.9131563295584044, 489.3642818721078243 ) ) ;
#13314 = ADVANCED_FACE ( 'NONE', ( #685 ), #3600, .F. ) ;
#13315 =( GEOMETRIC_REPRESENTATION_CONTEXT ( 3 ) GLOBAL_UNCERTAINTY_ASSIGNED_CONTEXT ( ( #5600 ) ) GLOBAL_UNIT_ASSIGNED_CONTEXT ( ( #12950, #6658, #4030 ) ) REPRESENTATION_CONTEXT ( 'NONE', 'WORKASPACE' ) );
#13316 = FACE_OUTER_BOUND ( 'NONE', #1156, .T. ) ;
#13317 = CARTESIAN_POINT ( 'NONE',  ( 22.99999999999998224, 10.00000000000000000, -31.00000000000003197 ) ) ;
#13318 = AXIS2_PLACEMENT_3D ( 'NONE', #19930, #13862, #20131 ) ;
#13319 = ORIENTED_EDGE ( 'NONE', *, *, #13938, .T. ) ;
#13320 = ADVANCED_BREP_SHAPE_REPRESENTATION ( '', ( #1489, #2741 ), #13578 ) ;
#13321 =( GEOMETRIC_REPRESENTATION_CONTEXT ( 3 ) GLOBAL_UNCERTAINTY_ASSIGNED_CONTEXT ( ( #3929 ) ) GLOBAL_UNIT_ASSIGNED_CONTEXT ( ( #10782, #1481, #20139 ) ) REPRESENTATION_CONTEXT ( 'NONE', 'WORKASPACE' ) );
#13322 = PRESENTATION_LAYER_ASSIGNMENT (  '', '', ( #19531 ) ) ;
#13323 = ORIENTED_EDGE ( 'NONE', *, *, #8790, .T. ) ;
#13324 = AXIS2_PLACEMENT_3D ( 'NONE', #3855, #7053, #5588 ) ;
#13325 = CARTESIAN_POINT ( 'NONE',  ( 3.674999999999999822, -14.43750000000000000, -1.768083816268991068E-15 ) ) ;
#13326 = ORIENTED_EDGE ( 'NONE', *, *, #150, .F. ) ;
#13327 = EDGE_LOOP ( 'NONE', ( #9517, #12257, #11167, #11138 ) ) ;
#13328 = VECTOR ( 'NONE', #723, 1000.000000000000000 ) ;
#13329 = DIRECTION ( 'NONE',  ( -0.000000000000000000, -1.000000000000000000, -0.000000000000000000 ) ) ;
#13330 = CYLINDRICAL_SURFACE ( 'NONE', #9251, 10.00000000000000888 ) ;
#13331 = VECTOR ( 'NONE', #6607, 1000.000000000000000 ) ;
#13332 = SURFACE_SIDE_STYLE ('',( #7235 ) ) ;
#13333 = ORIENTED_EDGE ( 'NONE', *, *, #6771, .F. ) ;
#13334 = VECTOR ( 'NONE', #4058, 1000.000000000000227 ) ;
#13335 = DIRECTION ( 'NONE',  ( 1.000000000000000000, -0.000000000000000000, -7.715811803773179210E-14 ) ) ;
#13336 = DIRECTION ( 'NONE',  ( -0.000000000000000000, 1.000000000000000000, -0.000000000000000000 ) ) ;
#13337 = DIRECTION ( 'NONE',  ( 0.000000000000000000, 1.000000000000000000, -0.000000000000000000 ) ) ;
#13338 = EDGE_CURVE ( 'NONE', #4150, #3254, #16552, .T. ) ;
#13339 = VECTOR ( 'NONE', #7563, 1000.000000000000000 ) ;
#13340 = VECTOR ( 'NONE', #12601, 1000.000000000000000 ) ;
#13341 = CYLINDRICAL_SURFACE ( 'NONE', #5786, 10.00000000000000888 ) ;
#13342 = CARTESIAN_POINT ( 'NONE',  ( -211.5106270998635409, 113.1299228374912502, 29.36128450348865471 ) ) ;
#13343 = CARTESIAN_POINT ( 'NONE',  ( 40.00000000000001421, 5.000000000000000888, 0.000000000000000000 ) ) ;
#13344 = PLANE ( 'NONE',  #9710 ) ;
#13345 = EDGE_CURVE ( 'NONE', #6404, #10287, #8235, .T. ) ;
#13346 = ORIENTED_EDGE ( 'NONE', *, *, #10250, .T. ) ;
#13347 = CARTESIAN_POINT ( 'NONE',  ( 1.209468180989048008E-15, 2.719172340231729715E-32, 12.50000000000000000 ) ) ;
#13348 = DIRECTION ( 'NONE',  ( 1.000000000000000000, 5.889072920838430686E-16, -0.000000000000000000 ) ) ;
#13349 = EDGE_CURVE ( 'NONE', #7572, #7705, #14411, .T. ) ;
#13350 = CIRCLE ( 'NONE', #149, 10.00000000000000888 ) ;
#13351 = EDGE_LOOP ( 'NONE', ( #1975, #15977, #16047, #10899 ) ) ;
#13352 = PRESENTATION_LAYER_ASSIGNMENT (  '', '', ( #14640 ) ) ;
#13353 = CIRCLE ( 'NONE', #10372, 10.00000000000000888 ) ;
#13354 = ORIENTED_EDGE ( 'NONE', *, *, #10154, .F. ) ;
#13355 = AXIS2_PLACEMENT_3D ( 'NONE', #728, #19480, #18257 ) ;
#13356 = VERTEX_POINT ( 'NONE', #14616 ) ;
#13357 = MECHANICAL_DESIGN_GEOMETRIC_PRESENTATION_REPRESENTATION (  '', ( #8723 ), #11693 ) ;
#13358 = VECTOR ( 'NONE', #5558, 1000.000000000000000 ) ;
#13359 = ORIENTED_EDGE ( 'NONE', *, *, #12250, .F. ) ;
#13360 = DIRECTION ( 'NONE',  ( 6.123031769111888756E-17, -1.000000000000000000, -3.749151804555344967E-33 ) ) ;
#13361 = DIRECTION ( 'NONE',  ( 1.000000000000000000, 1.197852309262419498E-15, -0.000000000000000000 ) ) ;
#13362 = ORIENTED_EDGE ( 'NONE', *, *, #9456, .F. ) ;
#13363 = FACE_BOUND ( 'NONE', #6791, .T. ) ;
#13364 = DIRECTION ( 'NONE',  ( 9.815121534730717399E-17, -1.000000000000000000, 0.000000000000000000 ) ) ;
#13365 = COLOUR_RGB ( '', 0.31764706, 0.68627451, 0.89019608) ;
#13366 = UNCERTAINTY_MEASURE_WITH_UNIT (LENGTH_MEASURE( 1.000000000000000082E-05 ), #3122, 'distance_accuracy_value', 'NONE');
#13367 = AXIS2_PLACEMENT_3D ( 'NONE', #3242, #9521, #17150 ) ;
#13368 = FACE_OUTER_BOUND ( 'NONE', #11068, .T. ) ;
#13369 = DIRECTION ( 'NONE',  ( 1.000000000000000000, -0.000000000000000000, -0.000000000000000000 ) ) ;
#13370 = EDGE_CURVE ( 'NONE', #9751, #17102, #5678, .T. ) ;
#13371 = DIRECTION ( 'NONE',  ( -1.000000000000000000, -0.000000000000000000, -0.000000000000000000 ) ) ;
#13372 = ORIENTED_EDGE ( 'NONE', *, *, #2812, .F. ) ;
#13373 = DIRECTION ( 'NONE',  ( 0.000000000000000000, 0.000000000000000000, -1.000000000000000000 ) ) ;
#13374 = CARTESIAN_POINT ( 'NONE',  ( 133.4893729001365728, 80.91625508013694912, 0.000000000000000000 ) ) ;
#13375 = CARTESIAN_POINT ( 'NONE',  ( 10.00000000000000000, 0.000000000000000000, 0.000000000000000000 ) ) ;
#13376 = SURFACE_SIDE_STYLE ('',( #5223 ) ) ;
#13377 = EDGE_LOOP ( 'NONE', ( #16740, #872, #17016, #10121 ) ) ;
#13378 = ORIENTED_EDGE ( 'NONE', *, *, #7247, .F. ) ;
#13379 = AXIS2_PLACEMENT_3D ( 'NONE', #396, #19044, #14219 ) ;
#13380 = ORIENTED_EDGE ( 'NONE', *, *, #18466, .T. ) ;
#13381 = CIRCLE ( 'NONE', #4473, 17.52499999999999858 ) ;
#13382 = ORIENTED_EDGE ( 'NONE', *, *, #1941, .F. ) ;
#13383 = EDGE_LOOP ( 'NONE', ( #10817, #13062, #15531, #8604 ) ) ;
#13384 = PLANE ( 'NONE',  #2674 ) ;
#13385 = CARTESIAN_POINT ( 'NONE',  ( 31.00000000000003553, 19.00000000000000000, 25.99999999999999645 ) ) ;
#13386 = ORIENTED_EDGE ( 'NONE', *, *, #4825, .F. ) ;
#13387 = CARTESIAN_POINT ( 'NONE',  ( 463.8334540492693350, 191.8198460455371333, 225.0057801310552463 ) ) ;
#13388 = PRESENTATION_STYLE_ASSIGNMENT (( #15423 ) ) ;
#13389 =( NAMED_UNIT ( * ) SI_UNIT ( $, .STERADIAN. ) SOLID_ANGLE_UNIT ( ) );
#13390 = DIRECTION ( 'NONE',  ( 0.000000000000000000, 0.000000000000000000, 1.000000000000000000 ) ) ;
#13391 = VECTOR ( 'NONE', #2763, 1000.000000000000000 ) ;
#13392 = FACE_OUTER_BOUND ( 'NONE', #19689, .T. ) ;
#13393 = EDGE_CURVE ( 'NONE', #4349, #8344, #11738, .T. ) ;
#13394 = LINE ( 'NONE', #19632, #10794 ) ;
#13395 = DIRECTION ( 'NONE',  ( -1.000000000000000000, 0.000000000000000000, 0.000000000000000000 ) ) ;
#13396 = COLOUR_RGB ( '', 0.09019608, 0.27058824, 0.51372549) ;
#13397 = SURFACE_SIDE_STYLE ('',( #12127 ) ) ;
#13398 =( NAMED_UNIT ( * ) SI_UNIT ( $, .STERADIAN. ) SOLID_ANGLE_UNIT ( ) );
#13399 = PLANE ( 'NONE',  #4260 ) ;
#13400 = DIRECTION ( 'NONE',  ( 0.000000000000000000, 0.000000000000000000, 1.000000000000000000 ) ) ;
#13401 = ORIENTED_EDGE ( 'NONE', *, *, #7954, .T. ) ;
#13402 = ORIENTED_EDGE ( 'NONE', *, *, #12804, .F. ) ;
#13403 = UNCERTAINTY_MEASURE_WITH_UNIT (LENGTH_MEASURE( 1.000000000000000082E-05 ), #4395, 'distance_accuracy_value', 'NONE');
#13404 = ORIENTED_EDGE ( 'NONE', *, *, #3159, .T. ) ;
#13405 = VERTEX_POINT ( 'NONE', #16479 ) ;
#13406 = ADVANCED_FACE ( 'NONE', ( #3898 ), #1041, .T. ) ;
#13407 = PRESENTATION_STYLE_ASSIGNMENT (( #17813 ) ) ;
#13408 = VECTOR ( 'NONE', #7386, 1000.000000000000000 ) ;
#13409 = DIRECTION ( 'NONE',  ( -0.000000000000000000, 1.000000000000000000, -0.000000000000000000 ) ) ;
#13410 = PLANE ( 'NONE',  #18098 ) ;
#13411 = CARTESIAN_POINT ( 'NONE',  ( 40.00000000000000000, 0.000000000000000000, -25.99999999999999645 ) ) ;
#13412 = DIRECTION ( 'NONE',  ( 0.000000000000000000, 0.000000000000000000, -1.000000000000000000 ) ) ;
#13413 = LINE ( 'NONE', #11644, #15021 ) ;
#13414 = CARTESIAN_POINT ( 'NONE',  ( 31.00000000000000000, 8.000000000000000000, -21.00000000000000355 ) ) ;
#13415 = DIRECTION ( 'NONE',  ( 0.000000000000000000, 1.000000000000000000, 0.000000000000000000 ) ) ;
#13416 = CARTESIAN_POINT ( 'NONE',  ( -26.00000000000000000, 11.00000000000000000, -31.00000000000003908 ) ) ;
#13417 = CARTESIAN_POINT ( 'NONE',  ( -35.00000000000000000, 8.000000000000000000, 20.99999999999999289 ) ) ;
#13418 = DIRECTION ( 'NONE',  ( 0.000000000000000000, 0.7071067811865336949, -0.7071067811865614505 ) ) ;
#13419 = EDGE_CURVE ( 'NONE', #13936, #6580, #14890, .T. ) ;
#13420 = DIRECTION ( 'NONE',  ( 1.000000000000000000, 1.197852309262419498E-15, -0.000000000000000000 ) ) ;
#13421 = EDGE_CURVE ( 'NONE', #15933, #5629, #8446, .T. ) ;
#13422 = ORIENTED_EDGE ( 'NONE', *, *, #20093, .T. ) ;
#13423 = EDGE_CURVE ( 'NONE', #6600, #12374, #10085, .T. ) ;
#13424 = EDGE_LOOP ( 'NONE', ( #643, #18312, #17868, #8403 ) ) ;
#13425 =( LENGTH_UNIT ( ) NAMED_UNIT ( * ) SI_UNIT ( .MILLI., .METRE. ) );
#13426 = ORIENTED_EDGE ( 'NONE', *, *, #17711, .F. ) ;
#13427 = ORIENTED_EDGE ( 'NONE', *, *, #8291, .T. ) ;
#13428 = EDGE_CURVE ( 'NONE', #9757, #18631, #14722, .T. ) ;
#13429 = VERTEX_POINT ( 'NONE', #8524 ) ;
#13430 = DIRECTION ( 'NONE',  ( 0.000000000000000000, 0.000000000000000000, -1.000000000000000000 ) ) ;
#13431 = EDGE_CURVE ( 'NONE', #15689, #3089, #13585, .T. ) ;
#13432 = APPLICATION_CONTEXT ( 'automotive_design' ) ;
#13433 = CYLINDRICAL_SURFACE ( 'NONE', #12484, 10.00000000000000888 ) ;
#13434 = VERTEX_POINT ( 'NONE', #16091 ) ;
#13435 = PRESENTATION_STYLE_ASSIGNMENT (( #7045 ) ) ;
#13436 = DIRECTION ( 'NONE',  ( 0.000000000000000000, 1.000000000000000000, 0.000000000000000000 ) ) ;
#13437 = CARTESIAN_POINT ( 'NONE',  ( 423.8334540492694487, 191.8198460455371333, 81.76606011801540319 ) ) ;
#13438 = LINE ( 'NONE', #10434, #3047 ) ;
#13439 = LINE ( 'NONE', #16738, #5948 ) ;
#13440 = LINE ( 'NONE', #19676, #7098 ) ;
#13441 = EDGE_CURVE ( 'NONE', #12894, #14969, #8338, .T. ) ;
#13442 = VERTEX_POINT ( 'NONE', #590 ) ;
#13443 = CARTESIAN_POINT ( 'NONE',  ( 31.00000000000001776, 10.00000000000000000, -25.99999999999999645 ) ) ;
#13444 = COLOUR_RGB ( '', 0.08235294, 0.09019608, 0.10196078) ;
#13445 = FILL_AREA_STYLE_COLOUR ( '', #18218 ) ;
#13446 = VECTOR ( 'NONE', #18397, 1000.000000000000000 ) ;
#13447 = ADVANCED_FACE ( 'NONE', ( #5159 ), #11427, .F. ) ;
#13448 = ORIENTED_EDGE ( 'NONE', *, *, #5362, .T. ) ;
#13449 = ORIENTED_EDGE ( 'NONE', *, *, #1340, .F. ) ;
#13450 = EDGE_CURVE ( 'NONE', #16176, #18080, #7973, .T. ) ;
#13451 = ORIENTED_EDGE ( 'NONE', *, *, #5273, .F. ) ;
#13452 = SURFACE_STYLE_FILL_AREA ( #555 ) ;
#13453 = LINE ( 'NONE', #11797, #11184 ) ;
#13454 = UNCERTAINTY_MEASURE_WITH_UNIT (LENGTH_MEASURE( 1.000000000000000082E-05 ), #11249, 'distance_accuracy_value', 'NONE');
#13455 = ORIENTED_EDGE ( 'NONE', *, *, #2322, .F. ) ;
#13456 = CARTESIAN_POINT ( 'NONE',  ( 503.8334540492693918, 242.8734308960556234, 250.0000000000000000 ) ) ;
#13457 = FILL_AREA_STYLE_COLOUR ( '', #14271 ) ;
#13458 = CYLINDRICAL_SURFACE ( 'NONE', #7027, 10.00000000000000888 ) ;
#13459 = DIRECTION ( 'NONE',  ( 1.197852309262419498E-15, -1.000000000000000000, 0.000000000000000000 ) ) ;
#13460 = DIRECTION ( 'NONE',  ( 1.000000000000000000, 5.889072920838430686E-16, -0.000000000000000000 ) ) ;
#13461 = ORIENTED_EDGE ( 'NONE', *, *, #568, .F. ) ;
#13462 = PRESENTATION_STYLE_ASSIGNMENT (( #14889 ) ) ;
#13463 = DIRECTION ( 'NONE',  ( -0.000000000000000000, -0.000000000000000000, 1.000000000000000000 ) ) ;
#13464 = SHAPE_DEFINITION_REPRESENTATION ( #7782, #4054 ) ;
#13465 = ORIENTED_EDGE ( 'NONE', *, *, #10485, .T. ) ;
#13466 =( NAMED_UNIT ( * ) PLANE_ANGLE_UNIT ( ) SI_UNIT ( $, .RADIAN. ) );
#13467 = EDGE_CURVE ( 'NONE', #18235, #19590, #3695, .T. ) ;
#13468 = EDGE_LOOP ( 'NONE', ( #11612, #15410, #9589, #769 ) ) ;
#13469 = ORIENTED_EDGE ( 'NONE', *, *, #3219, .T. ) ;
#13470 = AXIS2_PLACEMENT_3D ( 'NONE', #17854, #5295, #636 ) ;
#13471 = VERTEX_POINT ( 'NONE', #13286 ) ;
#13472 = ADVANCED_FACE ( 'NONE', ( #2134, #19533, #6905, #13190, #5343, #2440 ), #19839, .T. ) ;
#13473 = VERTEX_POINT ( 'NONE', #5854 ) ;
#13474 = FACE_OUTER_BOUND ( 'NONE', #223, .T. ) ;
#13475 = CARTESIAN_POINT ( 'NONE',  ( 25.99999999999998224, 10.00000000000000000, -31.00000000000003197 ) ) ;
#13476 = ORIENTED_EDGE ( 'NONE', *, *, #8240, .T. ) ;
#13477 = CARTESIAN_POINT ( 'NONE',  ( 25.99999999999997868, 10.00000000000000000, 40.00000000000000711 ) ) ;
#13478 = FILL_AREA_STYLE ('',( #2219 ) ) ;
#13479 = LINE ( 'NONE', #1062, #7324 ) ;
#13480 = AXIS2_PLACEMENT_3D ( 'NONE', #16335, #19070, #3637 ) ;
#13481 = FILL_AREA_STYLE ('',( #1167 ) ) ;
#13482 = VECTOR ( 'NONE', #12192, 1000.000000000000000 ) ;
#13483 = CARTESIAN_POINT ( 'NONE',  ( -26.00000000000002842, 0.000000000000000000, -31.00000000000003197 ) ) ;
#13484 = CARTESIAN_POINT ( 'NONE',  ( -1.000000000000009104, 141.3905724437643414, 484.7051316060566819 ) ) ;
#13485 = FACE_OUTER_BOUND ( 'NONE', #17776, .T. ) ;
#13486 =( LENGTH_UNIT ( ) NAMED_UNIT ( * ) SI_UNIT ( .MILLI., .METRE. ) );
#13487 = CARTESIAN_POINT ( 'NONE',  ( -39.99999999999997868, 3.000000000000000000, -19.99999999999999645 ) ) ;
#13488 = DIRECTION ( 'NONE',  ( 0.000000000000000000, 0.000000000000000000, 1.000000000000000000 ) ) ;
#13489 = DIRECTION ( 'NONE',  ( 0.000000000000000000, 0.000000000000000000, -1.000000000000000000 ) ) ;
#13490 = EDGE_LOOP ( 'NONE', ( #6272, #12497 ) ) ;
#13491 = VECTOR ( 'NONE', #4398, 1000.000000000000000 ) ;
#13492 = EDGE_LOOP ( 'NONE', ( #11606, #19665, #15662, #12375, #5675, #12839, #11294, #8006, #4882, #2208, #9567, #14727 ) ) ;
#13493 = EDGE_CURVE ( 'NONE', #15757, #2216, #2642, .T. ) ;
#13494 = AXIS2_PLACEMENT_3D ( 'NONE', #8495, #10347, #16658 ) ;
#13495 = ORIENTED_EDGE ( 'NONE', *, *, #8362, .T. ) ;
#13496 = SURFACE_SIDE_STYLE ('',( #16402 ) ) ;
#13497 = CARTESIAN_POINT ( 'NONE',  ( 31.81980515339464333, 8.000000000000000000, 28.51980515339463906 ) ) ;
#13498 = DIRECTION ( 'NONE',  ( 0.000000000000000000, 1.000000000000000000, 0.000000000000000000 ) ) ;
#13499 = CARTESIAN_POINT ( 'NONE',  ( 111.4893729001366012, 127.7247684487574304, 368.0000000000000000 ) ) ;
#13500 = DIRECTION ( 'NONE',  ( 0.000000000000000000, 0.000000000000000000, -1.000000000000000000 ) ) ;
#13501 = LINE ( 'NONE', #3823, #7135 ) ;
#13502 = FILL_AREA_STYLE_COLOUR ( '', #17977 ) ;
#13503 = CARTESIAN_POINT ( 'NONE',  ( -39.99999999999999289, 11.00000000000000000, -26.00000000000000355 ) ) ;
#13504 = COLOUR_RGB ( '', 0.09019608, 0.27058824, 0.51372549) ;
#13505 = DIRECTION ( 'NONE',  ( -1.000000000000000000, 0.000000000000000000, 0.000000000000000000 ) ) ;
#13506 = AXIS2_PLACEMENT_3D ( 'NONE', #487, #17481, #11108 ) ;
#13507 = CARTESIAN_POINT ( 'NONE',  ( 22.99999999999998224, 6.000000000000000000, -36.99999999999999289 ) ) ;
#13508 = MECHANICAL_DESIGN_GEOMETRIC_PRESENTATION_REPRESENTATION (  '', ( #9545 ), #7253 ) ;
#13509 = SURFACE_SIDE_STYLE ('',( #18644 ) ) ;
#13510 = ADVANCED_FACE ( 'NONE', ( #8840 ), #5753, .F. ) ;
#13511 = DIRECTION ( 'NONE',  ( -0.000000000000000000, -0.000000000000000000, 1.000000000000000000 ) ) ;
#13512 = ORIENTED_EDGE ( 'NONE', *, *, #16906, .T. ) ;
#13513 = ORIENTED_EDGE ( 'NONE', *, *, #1586, .F. ) ;
#13514 = CARTESIAN_POINT ( 'NONE',  ( -26.00000000000002132, 10.00000000000000000, -31.00000000000003553 ) ) ;
#13515 = VERTEX_POINT ( 'NONE', #14924 ) ;
#13516 = ORIENTED_EDGE ( 'NONE', *, *, #5303, .T. ) ;
#13517 = AXIS2_PLACEMENT_3D ( 'NONE', #8185, #7024, #5660 ) ;
#13518 = ADVANCED_FACE ( 'NONE', ( #7200 ), #2541, .T. ) ;
#13519 = COLOUR_RGB ( '', 0.08235294, 0.09019608, 0.10196078) ;
#13520 = DIRECTION ( 'NONE',  ( -1.000000000000000000, 0.000000000000000000, 0.000000000000000000 ) ) ;
#13521 = DIRECTION ( 'NONE',  ( -1.000000000000000000, -0.000000000000000000, -0.000000000000000000 ) ) ;
#13522 = DIRECTION ( 'NONE',  ( -1.000000000000000000, 0.000000000000000000, 0.000000000000000000 ) ) ;
#13523 = ADVANCED_FACE ( 'NONE', ( #9039 ), #16988, .F. ) ;
#13524 = PRESENTATION_LAYER_ASSIGNMENT (  '', '', ( #17123 ) ) ;
#13525 = CARTESIAN_POINT ( 'NONE',  ( 19.99999999999995381, 3.000000000000000000, -39.99999999999999289 ) ) ;
#13526 = PRESENTATION_STYLE_ASSIGNMENT (( #919 ) ) ;
#13527 = CARTESIAN_POINT ( 'NONE',  ( -80.71908396425561705, 138.8395222545321133, 489.5364562303509501 ) ) ;
#13528 = EDGE_LOOP ( 'NONE', ( #7673, #372, #41, #7624 ) ) ;
#13529 = CARTESIAN_POINT ( 'NONE',  ( 0.000000000000000000, 0.000000000000000000, 0.000000000000000000 ) ) ;
#13530 = DIRECTION ( 'NONE',  ( -1.962615573354755500E-14, -0.7071067811865614505, -0.7071067811865336949 ) ) ;
#13531 = CARTESIAN_POINT ( 'NONE',  ( 1.347066989204613998E-15, 6.000000000000000000, 24.99999999999999645 ) ) ;
#13532 = AXIS2_PLACEMENT_3D ( 'NONE', #15943, #4412, #8099 ) ;
#13533 = EDGE_CURVE ( 'NONE', #11798, #13911, #8625, .T. ) ;
#13534 = VERTEX_POINT ( 'NONE', #4606 ) ;
#13535 = EDGE_CURVE ( 'NONE', #15750, #368, #9537, .T. ) ;
#13536 = VERTEX_POINT ( 'NONE', #4819 ) ;
#13537 = CARTESIAN_POINT ( 'NONE',  ( -23.00000000000002132, 0.000000000000000000, 37.00000000000000711 ) ) ;
#13538 = CARTESIAN_POINT ( 'NONE',  ( -1.734723475976807094E-15, 60.00000000000000711, 6.000000000000000000 ) ) ;
#13539 = ORIENTED_EDGE ( 'NONE', *, *, #150, .T. ) ;
#13540 = AXIS2_PLACEMENT_3D ( 'NONE', #18953, #15698, #20372 ) ;
#13541 = PLANE ( 'NONE',  #17094 ) ;
#13542 = CARTESIAN_POINT ( 'NONE',  ( -79.03224866309057006, 140.4930333293738727, 501.9895992312876274 ) ) ;
#13543 =( NAMED_UNIT ( * ) PLANE_ANGLE_UNIT ( ) SI_UNIT ( $, .RADIAN. ) );
#13544 = CARTESIAN_POINT ( 'NONE',  ( -21.85283368562565443, 319.7545334744432353, 489.0536462814662855 ) ) ;
#13545 = EDGE_CURVE ( 'NONE', #9428, #6211, #6026, .T. ) ;
#13546 = CARTESIAN_POINT ( 'NONE',  ( 25.99999999999997868, 0.000000000000000000, 40.00000000000000711 ) ) ;
#13547 = EDGE_CURVE ( 'NONE', #6655, #4371, #419, .T. ) ;
#13548 = FILL_AREA_STYLE_COLOUR ( '', #12143 ) ;
#13549 = CARTESIAN_POINT ( 'NONE',  ( -78.99999999999995737, 152.4824555358010798, 501.3921618609452366 ) ) ;
#13550 = VERTEX_POINT ( 'NONE', #7898 ) ;
#13551 = PLANE ( 'NONE',  #10207 ) ;
#13552 =( LENGTH_UNIT ( ) NAMED_UNIT ( * ) SI_UNIT ( .MILLI., .METRE. ) );
#13553 = APPLICATION_PROTOCOL_DEFINITION ( 'draft international standard', 'automotive_design', 1998, #12370 ) ;
#13554 = EDGE_CURVE ( 'NONE', #13107, #19851, #1689, .T. ) ;
#13555 = ORIENTED_EDGE ( 'NONE', *, *, #4117, .T. ) ;
#13556 = CARTESIAN_POINT ( 'NONE',  ( 111.4893729001366154, 77.72476844875745883, 250.0000000000000000 ) ) ;
#13557 = EDGE_CURVE ( 'NONE', #3628, #8580, #4050, .T. ) ;
#13558 = ORIENTED_EDGE ( 'NONE', *, *, #3595, .T. ) ;
#13559 = ORIENTED_EDGE ( 'NONE', *, *, #4504, .T. ) ;
#13560 = ORIENTED_EDGE ( 'NONE', *, *, #14045, .F. ) ;
#13561 = ADVANCED_BREP_SHAPE_REPRESENTATION ( '', ( #15204, #2741 ), #2413 ) ;
#13562 = CARTESIAN_POINT ( 'NONE',  ( -39.99999999999997868, 0.000000000000000000, -19.99999999999999645 ) ) ;
#13563 = EDGE_LOOP ( 'NONE', ( #14696, #2802 ) ) ;
#13564 = CARTESIAN_POINT ( 'NONE',  ( 53.48937290013659407, 145.9162550801369491, 250.0000000000000000 ) ) ;
#13565 = CARTESIAN_POINT ( 'NONE',  ( -1.242741617435013737E-14, 141.6406393683235194, 501.8237260975781737 ) ) ;
#13566 = ORIENTED_EDGE ( 'NONE', *, *, #14982, .T. ) ;
#13567 = FILL_AREA_STYLE ('',( #8614 ) ) ;
#13568 = DIRECTION ( 'NONE',  ( 1.387778780781446415E-16, -1.000000000000000000, 0.000000000000000000 ) ) ;
#13569 = TOROIDAL_SURFACE ( 'NONE', #18480, 8.000000000000000000, 1.000000000000000000 ) ;
#13570 = DIRECTION ( 'NONE',  ( 8.479266908829339085E-16, -1.000000000000000000, 0.000000000000000000 ) ) ;
#13571 = DIRECTION ( 'NONE',  ( 0.000000000000000000, 1.000000000000000000, 0.000000000000000000 ) ) ;
#13572 = CIRCLE ( 'NONE', #16536, 3.000000000000002665 ) ;
#13573 = CARTESIAN_POINT ( 'NONE',  ( 17.99999999999998579, 10.00000000000000000, -36.99999999999999289 ) ) ;
#13574 = EDGE_CURVE ( 'NONE', #15829, #12374, #3043, .T. ) ;
#13575 = DIRECTION ( 'NONE',  ( 1.000000000000000000, -0.000000000000000000, 0.000000000000000000 ) ) ;
#13576 = SHAPE_REPRESENTATION_RELATIONSHIP ( 'NONE' , 'NONE' ,  #1922, #4681 ) ;
#13577 = LINE ( 'NONE', #10172, #8736 ) ;
#13578 =( GEOMETRIC_REPRESENTATION_CONTEXT ( 3 ) GLOBAL_UNCERTAINTY_ASSIGNED_CONTEXT ( ( #11744 ) ) GLOBAL_UNIT_ASSIGNED_CONTEXT ( ( #16169, #2205, #2304 ) ) REPRESENTATION_CONTEXT ( 'NONE', 'WORKASPACE' ) );
#13579 = DIRECTION ( 'NONE',  ( 1.000000000000000000, 0.000000000000000000, 0.000000000000000000 ) ) ;
#13580 = EDGE_CURVE ( 'NONE', #13534, #14656, #8654, .T. ) ;
#13581 = VERTEX_POINT ( 'NONE', #13874 ) ;
#13582 = VECTOR ( 'NONE', #12556, 1000.000000000000000 ) ;
#13583 = ORIENTED_EDGE ( 'NONE', *, *, #18579, .T. ) ;
#13584 = EDGE_CURVE ( 'NONE', #5865, #11845, #20153, .T. ) ;
#13585 = CIRCLE ( 'NONE', #1355, 3.000000000000002665 ) ;
#13586 = UNCERTAINTY_MEASURE_WITH_UNIT (LENGTH_MEASURE( 1.000000000000000082E-05 ), #1262, 'distance_accuracy_value', 'NONE');
#13587 = VERTEX_POINT ( 'NONE', #10788 ) ;
#13588 = AXIS2_PLACEMENT_3D ( 'NONE', #15744, #15533, #14166 ) ;
#13589 = VERTEX_POINT ( 'NONE', #9137 ) ;
#13590 = CARTESIAN_POINT ( 'NONE',  ( -79.99999999999995737, 216.7545334744432921, 488.5655098179835818 ) ) ;
#13591 = CARTESIAN_POINT ( 'NONE',  ( 19.99999999999995381, 3.000000000000000000, -36.99999999999999289 ) ) ;
#13592 = DIRECTION ( 'NONE',  ( 0.000000000000000000, 1.000000000000000000, 0.000000000000000000 ) ) ;
#13593 =( GEOMETRIC_REPRESENTATION_CONTEXT ( 3 ) GLOBAL_UNCERTAINTY_ASSIGNED_CONTEXT ( ( #15235 ) ) GLOBAL_UNIT_ASSIGNED_CONTEXT ( ( #2718, #16668, #13849 ) ) REPRESENTATION_CONTEXT ( 'NONE', 'WORKASPACE' ) );
#13594 = DIRECTION ( 'NONE',  ( -3.854941057726255847E-16, -0.000000000000000000, 1.000000000000000000 ) ) ;
#13595 = CARTESIAN_POINT ( 'NONE',  ( -79.99999999999995737, 316.7545334744432921, 155.1946179577816167 ) ) ;
#13596 = DIRECTION ( 'NONE',  ( 0.000000000000000000, 0.000000000000000000, 1.000000000000000000 ) ) ;
#13597 = FACE_OUTER_BOUND ( 'NONE', #8776, .T. ) ;
#13598 = CIRCLE ( 'NONE', #4710, 10.00000000000000888 ) ;
#13599 = PRESENTATION_LAYER_ASSIGNMENT (  '', '', ( #748 ) ) ;
#13600 = FACE_OUTER_BOUND ( 'NONE', #5815, .T. ) ;
#13601 = SURFACE_STYLE_USAGE ( .BOTH. , #13793 ) ;
#13602 = DIRECTION ( 'NONE',  ( 0.000000000000000000, 0.000000000000000000, -1.000000000000000000 ) ) ;
#13603 = ADVANCED_FACE ( 'NONE', ( #8001, #6264, #15656, #1367, #13989, #20351 ), #10993, .F. ) ;
#13604 = DIRECTION ( 'NONE',  ( -1.000000000000000000, 0.000000000000000000, 1.450371633464475582E-15 ) ) ;
#13605 = CLOSED_SHELL ( 'NONE', ( #16547, #10935, #11689, #16487, #17188, #239, #5118, #17431, #18267, #15540, #8501, #6592, #9032, #8607, #19037, #1009, #18171, #17816, #14951, #2497, #7742, #6510 ) ) ;
#13606 = CIRCLE ( 'NONE', #13928, 18.50000000000000000 ) ;
#13607 = EDGE_LOOP ( 'NONE', ( #16929, #14548, #15830, #3453 ) ) ;
#13608 = DIRECTION ( 'NONE',  ( 1.450371633464484259E-15, 5.551115123125816150E-14, 1.000000000000000000 ) ) ;
#13609 = EDGE_LOOP ( 'NONE', ( #4794, #2256, #364, #19054 ) ) ;
#13610 = VERTEX_POINT ( 'NONE', #14180 ) ;
#13611 = COLOUR_RGB ( '', 0.66274510, 0.83137255, 0.94901961) ;
#13612 =( GEOMETRIC_REPRESENTATION_CONTEXT ( 3 ) GLOBAL_UNCERTAINTY_ASSIGNED_CONTEXT ( ( #8869 ) ) GLOBAL_UNIT_ASSIGNED_CONTEXT ( ( #17878, #463, #3670 ) ) REPRESENTATION_CONTEXT ( 'NONE', 'WORKASPACE' ) );
#13613 = SURFACE_STYLE_FILL_AREA ( #8405 ) ;
#13614 = AXIS2_PLACEMENT_3D ( 'NONE', #3820, #16405, #14827 ) ;
#13615 = UNCERTAINTY_MEASURE_WITH_UNIT (LENGTH_MEASURE( 1.000000000000000082E-05 ), #2939, 'distance_accuracy_value', 'NONE');
#13616 = DIRECTION ( 'NONE',  ( 0.000000000000000000, 0.000000000000000000, 1.000000000000000000 ) ) ;
#13617 =( GEOMETRIC_REPRESENTATION_CONTEXT ( 3 ) GLOBAL_UNCERTAINTY_ASSIGNED_CONTEXT ( ( #1028 ) ) GLOBAL_UNIT_ASSIGNED_CONTEXT ( ( #3866, #14879, #745 ) ) REPRESENTATION_CONTEXT ( 'NONE', 'WORKASPACE' ) );
#13618 = DIRECTION ( 'NONE',  ( 1.000000000000000000, 0.000000000000000000, 0.000000000000000000 ) ) ;
#13619 = CIRCLE ( 'NONE', #14603, 4.999999999999997335 ) ;
#13620 = AXIS2_PLACEMENT_3D ( 'NONE', #4804, #6551, #17451 ) ;
#13621 = FACE_OUTER_BOUND ( 'NONE', #5354, .T. ) ;
#13622 = CARTESIAN_POINT ( 'NONE',  ( -80.33253491209451624, 139.8177930281376291, 489.3130425433099049 ) ) ;
#13623 = CARTESIAN_POINT ( 'NONE',  ( 40.00000000000001421, 0.000000000000000000, 0.000000000000000000 ) ) ;
#13624 = ORIENTED_EDGE ( 'NONE', *, *, #4475, .T. ) ;
#13625 = LINE ( 'NONE', #18259, #17083 ) ;
#13626 = FACE_OUTER_BOUND ( 'NONE', #3289, .T. ) ;
#13627 = AXIS2_PLACEMENT_3D ( 'NONE', #1911, #15990, #19341 ) ;
#13628 = DIRECTION ( 'NONE',  ( 0.000000000000000000, 1.000000000000000000, 0.000000000000000000 ) ) ;
#13629 = MECHANICAL_DESIGN_GEOMETRIC_PRESENTATION_REPRESENTATION (  '', ( #17291 ), #8385 ) ;
#13630 = STYLED_ITEM ( 'NONE', ( #18354 ), #15739 ) ;
#13631 = PRESENTATION_LAYER_ASSIGNMENT (  '', '', ( #11000 ) ) ;
#13632 = ORIENTED_EDGE ( 'NONE', *, *, #3740, .T. ) ;
#13633 = VECTOR ( 'NONE', #13033, 1000.000000000000000 ) ;
#13634 = UNCERTAINTY_MEASURE_WITH_UNIT (LENGTH_MEASURE( 1.000000000000000082E-05 ), #14941, 'distance_accuracy_value', 'NONE');
#13635 = VERTEX_POINT ( 'NONE', #18803 ) ;
#13636 = EDGE_CURVE ( 'NONE', #11967, #8401, #14281, .T. ) ;
#13637 = AXIS2_PLACEMENT_3D ( 'NONE', #16875, #18193, #11831 ) ;
#13638 = DIRECTION ( 'NONE',  ( 0.000000000000000000, 1.000000000000000000, 0.000000000000000000 ) ) ;
#13639 = AXIS2_PLACEMENT_3D ( 'NONE', #1854, #17637, #3527 ) ;
#13640 = DIRECTION ( 'NONE',  ( -0.000000000000000000, -1.000000000000000000, -0.000000000000000000 ) ) ;
#13641 = UNCERTAINTY_MEASURE_WITH_UNIT (LENGTH_MEASURE( 1.000000000000000082E-05 ), #6012, 'distance_accuracy_value', 'NONE');
#13642 = STYLED_ITEM ( 'NONE', ( #103 ), #15010 ) ;
#13643 = EDGE_LOOP ( 'NONE', ( #11564, #13300, #11326, #15319 ) ) ;
#13644 = DIRECTION ( 'NONE',  ( 0.000000000000000000, 1.000000000000000000, 0.000000000000000000 ) ) ;
#13645 = DIRECTION ( 'NONE',  ( 1.000000000000000000, 0.000000000000000000, 0.000000000000000000 ) ) ;
#13646 = VECTOR ( 'NONE', #17514, 1000.000000000000000 ) ;
#13647 = DIRECTION ( 'NONE',  ( -1.000000000000000000, 0.000000000000000000, 0.000000000000000000 ) ) ;
#13648 = CARTESIAN_POINT ( 'NONE',  ( 6.649999999999999467, -18.17500000000000071, -2.225795557450314789E-15 ) ) ;
#13649 = DIRECTION ( 'NONE',  ( 0.000000000000000000, 0.000000000000000000, -1.000000000000000000 ) ) ;
#13650 = MECHANICAL_DESIGN_GEOMETRIC_PRESENTATION_REPRESENTATION (  '', ( #10039 ), #14637 ) ;
#13651 = DIRECTION ( 'NONE',  ( 0.000000000000000000, 0.000000000000000000, -1.000000000000000000 ) ) ;
#13652 = VECTOR ( 'NONE', #4923, 1000.000000000000000 ) ;
#13653 = ORIENTED_EDGE ( 'NONE', *, *, #6809, .F. ) ;
#13654 = CARTESIAN_POINT ( 'NONE',  ( 6.299999999999999822, 0.000000000000000000, 0.000000000000000000 ) ) ;
#13655 = FACE_OUTER_BOUND ( 'NONE', #9475, .T. ) ;
#13656 = SHAPE_DEFINITION_REPRESENTATION ( #14031, #16721 ) ;
#13657 = TOROIDAL_SURFACE ( 'NONE', #9049, 8.000000000000000000, 1.000000000000000000 ) ;
#13658 = EDGE_CURVE ( 'NONE', #15899, #15076, #17211, .T. ) ;
#13659 = VERTEX_POINT ( 'NONE', #7806 ) ;
#13660 = ORIENTED_EDGE ( 'NONE', *, *, #15566, .T. ) ;
#13661 = DIRECTION ( 'NONE',  ( 1.000000000000000000, 9.815121534730717399E-17, 0.000000000000000000 ) ) ;
#13662 = AXIS2_PLACEMENT_3D ( 'NONE', #3871, #1038, #13651 ) ;
#13663 = ORIENTED_EDGE ( 'NONE', *, *, #3429, .T. ) ;
#13664 = EDGE_LOOP ( 'NONE', ( #7059, #18182, #1233, #7871 ) ) ;
#13665 =( GEOMETRIC_REPRESENTATION_CONTEXT ( 3 ) GLOBAL_UNCERTAINTY_ASSIGNED_CONTEXT ( ( #8272 ) ) GLOBAL_UNIT_ASSIGNED_CONTEXT ( ( #16448, #16361, #17976 ) ) REPRESENTATION_CONTEXT ( 'NONE', 'WORKASPACE' ) );
#13666 = EDGE_CURVE ( 'NONE', #18338, #6397, #12757, .T. ) ;
#13667 = ORIENTED_EDGE ( 'NONE', *, *, #5776, .T. ) ;
#13668 = ADVANCED_FACE ( 'NONE', ( #19005 ), #5047, .T. ) ;
#13669 = AXIS2_PLACEMENT_3D ( 'NONE', #5184, #6736, #13026 ) ;
#13670 = DIRECTION ( 'NONE',  ( 0.000000000000000000, 0.000000000000000000, -1.000000000000000000 ) ) ;
#13671 = ORIENTED_EDGE ( 'NONE', *, *, #13907, .T. ) ;
#13672 = LINE ( 'NONE', #12116, #9775 ) ;
#13673 = EDGE_CURVE ( 'NONE', #2482, #504, #11277, .T. ) ;
#13674 =( LENGTH_UNIT ( ) NAMED_UNIT ( * ) SI_UNIT ( .MILLI., .METRE. ) );
#13675 = FILL_AREA_STYLE ('',( #18087 ) ) ;
#13676 = EDGE_CURVE ( 'NONE', #8577, #18077, #15904, .T. ) ;
#13677 = FACE_OUTER_BOUND ( 'NONE', #3653, .T. ) ;
#13678 =( NAMED_UNIT ( * ) SI_UNIT ( $, .STERADIAN. ) SOLID_ANGLE_UNIT ( ) );
#13679 = SURFACE_SIDE_STYLE ('',( #9029 ) ) ;
#13680 = LINE ( 'NONE', #12122, #4767 ) ;
#13681 = CARTESIAN_POINT ( 'NONE',  ( 39.99999999999999289, 8.000000000000000000, 18.99999999999999645 ) ) ;
#13682 = CARTESIAN_POINT ( 'NONE',  ( -26.00000000000000000, 19.00000000000000000, -31.00000000000003908 ) ) ;
#13683 = CARTESIAN_POINT ( 'NONE',  ( 40.00000000000000711, 19.00000000000000000, -26.00000000000000355 ) ) ;
#13684 =( NAMED_UNIT ( * ) PLANE_ANGLE_UNIT ( ) SI_UNIT ( $, .RADIAN. ) );
#13685 =( LENGTH_UNIT ( ) NAMED_UNIT ( * ) SI_UNIT ( .MILLI., .METRE. ) );
#13686 = VECTOR ( 'NONE', #15299, 1000.000000000000000 ) ;
#13687 = SURFACE_STYLE_USAGE ( .BOTH. , #1069 ) ;
#13688 = ADVANCED_FACE ( 'NONE', ( #4509 ), #20261, .T. ) ;
#13689 = DIRECTION ( 'NONE',  ( 0.000000000000000000, 0.000000000000000000, -1.000000000000000000 ) ) ;
#13690 = ORIENTED_EDGE ( 'NONE', *, *, #16216, .T. ) ;
#13691 = AXIS2_PLACEMENT_3D ( 'NONE', #10844, #17122, #7187 ) ;
#13692 = VERTEX_POINT ( 'NONE', #3366 ) ;
#13693 =( REPRESENTATION_RELATIONSHIP ('NONE','NONE', #12483, #11716 ) REPRESENTATION_RELATIONSHIP_WITH_TRANSFORMATION ( #1658 )SHAPE_REPRESENTATION_RELATIONSHIP( ) );
#13694 = ORIENTED_EDGE ( 'NONE', *, *, #12770, .T. ) ;
#13695 = EDGE_LOOP ( 'NONE', ( #107, #16809, #4490, #2926 ) ) ;
#13696 = EDGE_CURVE ( 'NONE', #305, #3170, #12956, .T. ) ;
#13697 = CARTESIAN_POINT ( 'NONE',  ( -79.72263070831506582, 138.8189518926663482, 489.9905112626940422 ) ) ;
#13698 = ORIENTED_EDGE ( 'NONE', *, *, #473, .F. ) ;
#13699 = CIRCLE ( 'NONE', #7456, 3.300000000000025135 ) ;
#13700 = DIRECTION ( 'NONE',  ( 0.000000000000000000, 0.000000000000000000, -1.000000000000000000 ) ) ;
#13701 =( LENGTH_UNIT ( ) NAMED_UNIT ( * ) SI_UNIT ( .MILLI., .METRE. ) );
#13702 = CARTESIAN_POINT ( 'NONE',  ( 88.88953019741013861, 80.91625508013694912, 245.0000000000000000 ) ) ;
#13703 = DIRECTION ( 'NONE',  ( 1.000000000000000000, 0.000000000000000000, 3.328238341717381552E-14 ) ) ;
#13704 = AXIS2_PLACEMENT_3D ( 'NONE', #1617, #6606, #12895 ) ;
#13705 = LINE ( 'NONE', #12458, #13391 ) ;
#13706 = LINE ( 'NONE', #15675, #1102 ) ;
#13707 = DIRECTION ( 'NONE',  ( 0.000000000000000000, 1.000000000000000000, 0.000000000000000000 ) ) ;
#13708 = PLANE ( 'NONE',  #7178 ) ;
#13709 =( NAMED_UNIT ( * ) PLANE_ANGLE_UNIT ( ) SI_UNIT ( $, .RADIAN. ) );
#13710 =( NAMED_UNIT ( * ) SI_UNIT ( $, .STERADIAN. ) SOLID_ANGLE_UNIT ( ) );
#13712 = CARTESIAN_POINT ( 'NONE',  ( 423.8334540492694487, 191.8198460455371333, 81.76606011801540319 ) ) ;
#13711 = MECHANICAL_DESIGN_GEOMETRIC_PRESENTATION_REPRESENTATION (  '', ( #19804 ), #18957 ) ;
#13713 = CARTESIAN_POINT ( 'NONE',  ( 493.8117674897343363, 134.2156642432025251, 245.0000000000000000 ) ) ;
#13714 = CIRCLE ( 'NONE', #16685, 3.300000000000011369 ) ;
#13715 = EDGE_CURVE ( 'NONE', #9425, #7477, #5020, .T. ) ;
#13716 = PRESENTATION_LAYER_ASSIGNMENT (  '', '', ( #4179 ) ) ;
#13717 = ORIENTED_EDGE ( 'NONE', *, *, #8591, .T. ) ;
#13718 = DIRECTION ( 'NONE',  ( 0.000000000000000000, 0.000000000000000000, -1.000000000000000000 ) ) ;
#13719 = VERTEX_POINT ( 'NONE', #9642 ) ;
#13720 = ORIENTED_EDGE ( 'NONE', *, *, #440, .F. ) ;
#13721 = LINE ( 'NONE', #1207, #2080 ) ;
#13722 = DIRECTION ( 'NONE',  ( -1.156482317317875275E-15, 0.000000000000000000, -1.000000000000000000 ) ) ;
#13723 = CARTESIAN_POINT ( 'NONE',  ( -32.00000000000000711, 10.00000000000000000, -22.00000000000000355 ) ) ;
#13724 = FILL_AREA_STYLE_COLOUR ( '', #1150 ) ;
#13725 = LINE ( 'NONE', #4247, #793 ) ;
#13726 =( NAMED_UNIT ( * ) SI_UNIT ( $, .STERADIAN. ) SOLID_ANGLE_UNIT ( ) );
#13727 = DIRECTION ( 'NONE',  ( -1.156482317317870344E-15, 0.000000000000000000, 1.000000000000000000 ) ) ;
#13728 = LINE ( 'NONE', #12273, #3813 ) ;
#13729 = FACE_OUTER_BOUND ( 'NONE', #14111, .T. ) ;
#13730 = DIRECTION ( 'NONE',  ( 0.000000000000000000, 0.000000000000000000, 1.000000000000000000 ) ) ;
#13731 = ORIENTED_EDGE ( 'NONE', *, *, #8300, .F. ) ;
#13732 = CARTESIAN_POINT ( 'NONE',  ( 0.000000000000000000, 309.2289037985885898, -86.48019484660916589 ) ) ;
#13733 = DIRECTION ( 'NONE',  ( 0.000000000000000000, 0.000000000000000000, 1.000000000000000000 ) ) ;
#13734 = AXIS2_PLACEMENT_3D ( 'NONE', #2467, #16410, #10298 ) ;
#13735 = VERTEX_POINT ( 'NONE', #15963 ) ;
#13736 = EDGE_CURVE ( 'NONE', #14418, #11558, #16129, .T. ) ;
#13737 = VERTEX_POINT ( 'NONE', #629 ) ;
#13738 = DIRECTION ( 'NONE',  ( 0.000000000000000000, 1.000000000000000000, 0.000000000000000000 ) ) ;
#13739 = VERTEX_POINT ( 'NONE', #14665 ) ;
#13740 = DIRECTION ( 'NONE',  ( 0.000000000000000000, 0.000000000000000000, 1.000000000000000000 ) ) ;
#13741 = LINE ( 'NONE', #13837, #9674 ) ;
#13742 = DIRECTION ( 'NONE',  ( 1.000000000000000000, 0.000000000000000000, 8.673617379884027583E-16 ) ) ;
#13743 = CARTESIAN_POINT ( 'NONE',  ( -21.00000000000002842, 0.000000000000000000, -32.49999999999999289 ) ) ;
#13744 =( NAMED_UNIT ( * ) SI_UNIT ( $, .STERADIAN. ) SOLID_ANGLE_UNIT ( ) );
#13745 = DIRECTION ( 'NONE',  ( -0.000000000000000000, -1.000000000000000000, -0.000000000000000000 ) ) ;
#13746 = AXIS2_PLACEMENT_3D ( 'NONE', #16389, #3989, #13099 ) ;
#13747 = EDGE_LOOP ( 'NONE', ( #11631, #10059, #14159, #20071 ) ) ;
#13748 = FILL_AREA_STYLE ('',( #13845 ) ) ;
#13749 = FACE_BOUND ( 'NONE', #762, .T. ) ;
#13750 = FACE_BOUND ( 'NONE', #7995, .T. ) ;
#13751 = ORIENTED_EDGE ( 'NONE', *, *, #14628, .F. ) ;
#13752 = ORIENTED_EDGE ( 'NONE', *, *, #13673, .T. ) ;
#13753 = EDGE_CURVE ( 'NONE', #9120, #11912, #1959, .T. ) ;
#13754 = ORIENTED_EDGE ( 'NONE', *, *, #1268, .F. ) ;
#13755 = EDGE_LOOP ( 'NONE', ( #19141, #19439, #1542, #19465, #17078, #9515 ) ) ;
#13756 = EDGE_LOOP ( 'NONE', ( #15712, #1589, #4797, #999 ) ) ;
#13757 = CARTESIAN_POINT ( 'NONE',  ( -44.50085094405407915, 159.0821755739672483, 505.3921618609452935 ) ) ;
#13758 = ORIENTED_EDGE ( 'NONE', *, *, #3811, .F. ) ;
#13759 = DIRECTION ( 'NONE',  ( 0.000000000000000000, 1.000000000000000000, 0.000000000000000000 ) ) ;
#13760 = VERTEX_POINT ( 'NONE', #537 ) ;
#13761 = CARTESIAN_POINT ( 'NONE',  ( 53.48937290013658696, 103.1299228374913923, 79.58252780074349175 ) ) ;
#13762 = EDGE_CURVE ( 'NONE', #503, #17973, #8280, .T. ) ;
#13763 =( NAMED_UNIT ( * ) SI_UNIT ( $, .STERADIAN. ) SOLID_ANGLE_UNIT ( ) );
#13764 = CARTESIAN_POINT ( 'NONE',  ( 2.625000000000000000, 14.59999999999999964, 0.000000000000000000 ) ) ;
#13765 = SURFACE_STYLE_FILL_AREA ( #15329 ) ;
#13766 = DIRECTION ( 'NONE',  ( 1.000000000000000000, 2.135044278125300850E-16, -0.000000000000000000 ) ) ;
#13767 = CARTESIAN_POINT ( 'NONE',  ( -1.000000000000007550, 146.1184945051222428, 479.9772095446988374 ) ) ;
#13768 = EDGE_CURVE ( 'NONE', #11636, #11158, #6699, .T. ) ;
#13769 = LINE ( 'NONE', #2538, #12447 ) ;
#13770 = DIRECTION ( 'NONE',  ( 0.000000000000000000, 0.000000000000000000, 1.000000000000000000 ) ) ;
#13771 = SURFACE_STYLE_USAGE ( .BOTH. , #13397 ) ;
#13772 = CARTESIAN_POINT ( 'NONE',  ( 0.000000000000000000, 301.0487089519826327, 2.148629195649657075E-12 ) ) ;
#13773 = LINE ( 'NONE', #7406, #10860 ) ;
#13774 = ORIENTED_EDGE ( 'NONE', *, *, #10472, .T. ) ;
#13775 = EDGE_CURVE ( 'NONE', #16217, #13442, #18184, .T. ) ;
#13776 = EDGE_CURVE ( 'NONE', #11810, #5165, #9921, .T. ) ;
#13777 = ORIENTED_EDGE ( 'NONE', *, *, #1044, .T. ) ;
#13778 = ORIENTED_EDGE ( 'NONE', *, *, #4308, .T. ) ;
#13779 = ORIENTED_EDGE ( 'NONE', *, *, #3969, .T. ) ;
#13780 =( NAMED_UNIT ( * ) SI_UNIT ( $, .STERADIAN. ) SOLID_ANGLE_UNIT ( ) );
#13781 = ORIENTED_EDGE ( 'NONE', *, *, #18220, .F. ) ;
#13782 = DIRECTION ( 'NONE',  ( 1.000000000000000000, 0.000000000000000000, 0.000000000000000000 ) ) ;
#13783 = EDGE_CURVE ( 'NONE', #19948, #17281, #19475, .T. ) ;
#13784 = STYLED_ITEM ( 'NONE', ( #5587 ), #5113 ) ;
#13785 = CARTESIAN_POINT ( 'NONE',  ( -25.99999999999999645, 68.00000000000000000, 31.00000000000003908 ) ) ;
#13786 = COLOUR_RGB ( '', 0.40784314, 0.44705882, 0.49803922) ;
#13787 = ORIENTED_EDGE ( 'NONE', *, *, #9857, .T. ) ;
#13788 = FACE_BOUND ( 'NONE', #12785, .T. ) ;
#13789 = CARTESIAN_POINT ( 'NONE',  ( -211.5106270998635409, 113.1299228374912502, 170.4174721992565082 ) ) ;
#13790 = DIRECTION ( 'NONE',  ( 1.000000000000000000, -0.000000000000000000, -0.000000000000000000 ) ) ;
#13791 = DIRECTION ( 'NONE',  ( 0.9999937692730440641, -0.003530072958125829961, 4.323092548925426475E-19 ) ) ;
#13792 = CARTESIAN_POINT ( 'NONE',  ( 35.00000000000000711, 0.000000000000000000, -35.00000000000000711 ) ) ;
#13793 = SURFACE_SIDE_STYLE ('',( #15050 ) ) ;
#13794 = ADVANCED_FACE ( 'NONE', ( #17844 ), #16426, .T. ) ;
#13795 = CARTESIAN_POINT ( 'NONE',  ( -31.00000000000000000, 11.00000000000000000, 25.99999999999999645 ) ) ;
#13796 = SURFACE_STYLE_USAGE ( .BOTH. , #5881 ) ;
#13797 = EDGE_CURVE ( 'NONE', #11717, #17622, #5696, .T. ) ;
#13798 = SHAPE_REPRESENTATION ( 'Part15', ( #2741 ), #13578 ) ;
#13799 = VECTOR ( 'NONE', #20274, 1000.000000000000000 ) ;
#13800 = CIRCLE ( 'NONE', #15134, 4.999999999999997335 ) ;
#13801 = AXIS2_PLACEMENT_3D ( 'NONE', #5846, #7688, #5744 ) ;
#13802 = VERTEX_POINT ( 'NONE', #8381 ) ;
#13803 = ORIENTED_EDGE ( 'NONE', *, *, #8489, .F. ) ;
#13804 = ORIENTED_EDGE ( 'NONE', *, *, #8164, .T. ) ;
#13805 = FACE_BOUND ( 'NONE', #16262, .T. ) ;
#13806 = ORIENTED_EDGE ( 'NONE', *, *, #16568, .F. ) ;
#13807 = EDGE_LOOP ( 'NONE', ( #11690, #13555 ) ) ;
#13808 = DIRECTION ( 'NONE',  ( -1.000000000000000000, -0.000000000000000000, -0.000000000000000000 ) ) ;
#13809 = DIRECTION ( 'NONE',  ( -1.000000000000000000, -0.000000000000000000, -0.000000000000000000 ) ) ;
#13810 = UNCERTAINTY_MEASURE_WITH_UNIT (LENGTH_MEASURE( 1.000000000000000082E-05 ), #8162, 'distance_accuracy_value', 'NONE');
#13811 = CARTESIAN_POINT ( 'NONE',  ( -118.0000000000000284, 316.7545334744432921, 205.1946179577815883 ) ) ;
#13812 = DIRECTION ( 'NONE',  ( 0.000000000000000000, 1.000000000000000000, 0.000000000000000000 ) ) ;
#13813 = COLOUR_RGB ( '', 0.31764706, 0.68627451, 0.89019608) ;
#13814 = SURFACE_STYLE_FILL_AREA ( #1422 ) ;
#13815 = VECTOR ( 'NONE', #14806, 1000.000000000000000 ) ;
#13816 = PRESENTATION_STYLE_ASSIGNMENT (( #10621 ) ) ;
#13817 = LINE ( 'NONE', #18249, #1733 ) ;
#13818 = STYLED_ITEM ( 'NONE', ( #18462 ), #5969 ) ;
#13819 = EDGE_CURVE ( 'NONE', #16767, #18834, #13598, .T. ) ;
#13820 = LINE ( 'NONE', #20197, #1051 ) ;
#13821 = DIRECTION ( 'NONE',  ( 1.000000000000000000, 0.000000000000000000, 0.000000000000000000 ) ) ;
#13822 = LINE ( 'NONE', #2586, #13909 ) ;
#13823 = CARTESIAN_POINT ( 'NONE',  ( -0.8168643132833559584, 140.1532854590085435, 501.4923746928197943 ) ) ;
#13824 = ORIENTED_EDGE ( 'NONE', *, *, #13056, .F. ) ;
#13825 = FILL_AREA_STYLE_COLOUR ( '', #19219 ) ;
#13826 = EDGE_CURVE ( 'NONE', #18923, #2094, #16033, .T. ) ;
#13827 = SURFACE_STYLE_USAGE ( .BOTH. , #10535 ) ;
#13828 = EDGE_CURVE ( 'NONE', #14969, #1468, #81, .T. ) ;
#13829 = AXIS2_PLACEMENT_3D ( 'NONE', #17538, #3916, #3439 ) ;
#13830 = COLOUR_RGB ( '', 0.72549020, 0.75294118, 0.79215686) ;
#13831 = VERTEX_POINT ( 'NONE', #5390 ) ;
#13832 = ORIENTED_EDGE ( 'NONE', *, *, #14677, .F. ) ;
#13833 = DIRECTION ( 'NONE',  ( 1.000000000000000000, 0.000000000000000000, 0.000000000000000000 ) ) ;
#13834 = FACE_OUTER_BOUND ( 'NONE', #15865, .T. ) ;
#13835 = ORIENTED_EDGE ( 'NONE', *, *, #18821, .F. ) ;
#13836 = DIRECTION ( 'NONE',  ( 0.000000000000000000, 1.000000000000000000, 0.000000000000000000 ) ) ;
#13837 = CARTESIAN_POINT ( 'NONE',  ( -26.00000000000000000, 19.00000000000000000, -40.00000000000000711 ) ) ;
#13838 = CIRCLE ( 'NONE', #17452, 3.000000000000002665 ) ;
#13839 = CARTESIAN_POINT ( 'NONE',  ( -79.99999999999994316, 141.4904453270995646, 501.7347375422862683 ) ) ;
#13840 = VECTOR ( 'NONE', #12595, 1000.000000000000000 ) ;
#13841 = PLANE ( 'NONE',  #8824 ) ;
#13842 = STYLED_ITEM ( 'NONE', ( #6087 ), #16082 ) ;
#13843 = CARTESIAN_POINT ( 'NONE',  ( 503.8334540492693918, 191.8198460455371333, 158.2339398819845826 ) ) ;
#13844 = ORIENTED_EDGE ( 'NONE', *, *, #816, .T. ) ;
#13845 = FILL_AREA_STYLE_COLOUR ( '', #16431 ) ;
#13846 = ORIENTED_EDGE ( 'NONE', *, *, #2291, .T. ) ;
#13847 = FACE_OUTER_BOUND ( 'NONE', #10257, .T. ) ;
#13848 = SURFACE_STYLE_FILL_AREA ( #7568 ) ;
#13849 =( NAMED_UNIT ( * ) SI_UNIT ( $, .STERADIAN. ) SOLID_ANGLE_UNIT ( ) );
#13850 = PRODUCT_DEFINITION_SHAPE ( 'NONE', 'NONE',  #20386 ) ;
#13851 = EDGE_CURVE ( 'NONE', #18631, #19010, #11672, .T. ) ;
#13852 = ORIENTED_EDGE ( 'NONE', *, *, #18776, .T. ) ;
#13853 = AXIS2_PLACEMENT_3D ( 'NONE', #2562, #19865, #13418 ) ;
#13854 = VERTEX_POINT ( 'NONE', #3845 ) ;
#13855 = ORIENTED_EDGE ( 'NONE', *, *, #8400, .T. ) ;
#13856 = ORIENTED_EDGE ( 'NONE', *, *, #1020, .T. ) ;
#13857 = MECHANICAL_DESIGN_GEOMETRIC_PRESENTATION_REPRESENTATION (  '', ( #5961 ), #4032 ) ;
#13858 = MECHANICAL_DESIGN_GEOMETRIC_PRESENTATION_REPRESENTATION (  '', ( #3992 ), #5640 ) ;
#13859 =( GEOMETRIC_REPRESENTATION_CONTEXT ( 3 ) GLOBAL_UNCERTAINTY_ASSIGNED_CONTEXT ( ( #8891 ) ) GLOBAL_UNIT_ASSIGNED_CONTEXT ( ( #7145, #11559, #8784 ) ) REPRESENTATION_CONTEXT ( 'NONE', 'WORKASPACE' ) );
#13860 = CARTESIAN_POINT ( 'NONE',  ( 0.000000000000000000, 138.7545334744432637, 500.3921618609452366 ) ) ;
#13861 = ORIENTED_EDGE ( 'NONE', *, *, #7640, .F. ) ;
#13862 = DIRECTION ( 'NONE',  ( -1.000000000000000000, 0.000000000000000000, 1.156482317317881191E-15 ) ) ;
#13863 =( NAMED_UNIT ( * ) SI_UNIT ( $, .STERADIAN. ) SOLID_ANGLE_UNIT ( ) );
#13864 = CARTESIAN_POINT ( 'NONE',  ( -211.5106270998635409, 113.1299228374912502, 79.58252780074349175 ) ) ;
#13865 =( NAMED_UNIT ( * ) PLANE_ANGLE_UNIT ( ) SI_UNIT ( $, .RADIAN. ) );
#13866 = EDGE_CURVE ( 'NONE', #14767, #10724, #7989, .T. ) ;
#13867 = DIRECTION ( 'NONE',  ( 3.854941057726254860E-16, 0.000000000000000000, -1.000000000000000000 ) ) ;
#13868 = CARTESIAN_POINT ( 'NONE',  ( -44.50085094405410757, 209.4098724938429541, 505.3921618609452935 ) ) ;
#13869 = CARTESIAN_POINT ( 'NONE',  ( 2.265596578422603396E-15, -3.000000000000000000, 18.50000000000000000 ) ) ;
#13870 = CARTESIAN_POINT ( 'NONE',  ( -79.99999999999995737, 152.4824555358010798, 501.3921618609452366 ) ) ;
#13871 = AXIS2_PLACEMENT_3D ( 'NONE', #16372, #11406, #3776 ) ;
#13872 = LINE ( 'NONE', #10786, #6701 ) ;
#13873 = DIRECTION ( 'NONE',  ( 1.000000000000000000, 0.000000000000000000, -0.000000000000000000 ) ) ;
#13874 = CARTESIAN_POINT ( 'NONE',  ( 475.8334540492694487, 214.2156642432025251, 245.0000000000000000 ) ) ;
#13875 = FACE_OUTER_BOUND ( 'NONE', #14442, .T. ) ;
#13876 = CARTESIAN_POINT ( 'NONE',  ( 30.99999999999996092, 3.000000000000000000, -30.99999999999999289 ) ) ;
#13877 = DIRECTION ( 'NONE',  ( 0.000000000000000000, 1.000000000000000000, -1.224646799147353207E-16 ) ) ;
#13878 = EDGE_LOOP ( 'NONE', ( #6550, #7277, #4410, #44 ) ) ;
#13879 = EDGE_CURVE ( 'NONE', #7546, #15663, #14859, .T. ) ;
#13880 = VERTEX_POINT ( 'NONE', #19585 ) ;
#13881 = PRODUCT_DEFINITION ( 'UNKNOWN', '', #14231, #3905 ) ;
#13882 = VERTEX_POINT ( 'NONE', #6636 ) ;
#13883 = EDGE_LOOP ( 'NONE', ( #386, #18839, #13901, #3661, #3404, #6574 ) ) ;
#13884 = DIRECTION ( 'NONE',  ( 1.000000000000000000, 0.000000000000000000, 0.000000000000000000 ) ) ;
#13885 = ORIENTED_EDGE ( 'NONE', *, *, #16689, .T. ) ;
#13886 = ADVANCED_FACE ( 'NONE', ( #17532 ), #5087, .T. ) ;
#13887 = DIRECTION ( 'NONE',  ( -6.123031769111888756E-17, 1.000000000000000000, 3.749151804555344967E-33 ) ) ;
#13888 = LINE ( 'NONE', #6078, #16001 ) ;
#13889 = CARTESIAN_POINT ( 'NONE',  ( -3.000000000000003109, 60.00000000000000711, 9.013878188659973034 ) ) ;
#13890 = VECTOR ( 'NONE', #2011, 1000.000000000000000 ) ;
#13891 = SURFACE_STYLE_USAGE ( .BOTH. , #18523 ) ;
#13892 = EDGE_CURVE ( 'NONE', #17086, #16276, #917, .T. ) ;
#13893 = LINE ( 'NONE', #5970, #3418 ) ;
#13894 = CARTESIAN_POINT ( 'NONE',  ( -31.00000000000002842, 3.000000000000000000, 31.00000000000000000 ) ) ;
#13895 = CARTESIAN_POINT ( 'NONE',  ( 31.00000000000003553, 10.00000000000000000, -23.00000000000000000 ) ) ;
#13896 = FACE_OUTER_BOUND ( 'NONE', #11535, .T. ) ;
#13897 = FILL_AREA_STYLE ('',( #19969 ) ) ;
#13898 = PRESENTATION_LAYER_ASSIGNMENT (  '', '', ( #15894 ) ) ;
#13899 = EDGE_CURVE ( 'NONE', #13165, #4285, #8678, .T. ) ;
#13900 = EDGE_CURVE ( 'NONE', #17522, #2504, #7240, .T. ) ;
#13901 = ORIENTED_EDGE ( 'NONE', *, *, #1034, .F. ) ;
#13902 = VERTEX_POINT ( 'NONE', #5683 ) ;
#13903 = ORIENTED_EDGE ( 'NONE', *, *, #9345, .F. ) ;
#13904 = ORIENTED_EDGE ( 'NONE', *, *, #18776, .F. ) ;
#13905 = PRODUCT_DEFINITION_FORMATION_WITH_SPECIFIED_SOURCE ( 'ANY', '', #15518, .NOT_KNOWN. ) ;
#13906 = MECHANICAL_DESIGN_GEOMETRIC_PRESENTATION_REPRESENTATION (  '', ( #8980 ), #16562 ) ;
#13907 = EDGE_CURVE ( 'NONE', #12891, #1279, #12280, .T. ) ;
#13908 = ORIENTED_EDGE ( 'NONE', *, *, #2838, .T. ) ;
#13909 = VECTOR ( 'NONE', #12274, 1000.000000000000000 ) ;
#13910 = ORIENTED_EDGE ( 'NONE', *, *, #3173, .F. ) ;
#13911 = VERTEX_POINT ( 'NONE', #15380 ) ;
#13912 = DIRECTION ( 'NONE',  ( 0.000000000000000000, 1.000000000000000000, 0.000000000000000000 ) ) ;
#13913 = EDGE_CURVE ( 'NONE', #18235, #19815, #15251, .T. ) ;
#13914 = CARTESIAN_POINT ( 'NONE',  ( -22.00000000000001776, 8.000000000000000000, 33.00000000000000711 ) ) ;
#13915 = DIRECTION ( 'NONE',  ( 1.025567617263343161E-15, 0.7071067811865455743, 0.7071067811865494601 ) ) ;
#13916 = AXIS2_PLACEMENT_3D ( 'NONE', #1806, #8116, #14388 ) ;
#13917 = COLOUR_RGB ( '', 0.40784314, 0.44705882, 0.49803922) ;
#13918 = DIRECTION ( 'NONE',  ( 0.000000000000000000, 0.000000000000000000, -1.000000000000000000 ) ) ;
#13919 = EDGE_CURVE ( 'NONE', #10613, #2165, #18204, .T. ) ;
#13920 = CARTESIAN_POINT ( 'NONE',  ( 53.48937290013658696, 123.1299228374914065, 220.6387154965113382 ) ) ;
#13921 = CARTESIAN_POINT ( 'NONE',  ( -37.00000000000000000, 0.000000000000000000, 23.00000000000000355 ) ) ;
#13922 = ADVANCED_FACE ( 'NONE', ( #8788 ), #4159, .T. ) ;
#13923 = FACE_OUTER_BOUND ( 'NONE', #12652, .T. ) ;
#13924 =( BOUNDED_CURVE ( )  B_SPLINE_CURVE ( 3, ( #20281, #7824, #193, #1716 ),
 .UNSPECIFIED., .F., .T. ) 
 B_SPLINE_CURVE_WITH_KNOTS ( ( 4, 4 ),
 ( 0.000000000000000000, 1.570796326794907438 ),
 .UNSPECIFIED. ) 
 CURVE ( )  GEOMETRIC_REPRESENTATION_ITEM ( )  RATIONAL_B_SPLINE_CURVE ( ( 1.000000000000000000, 0.8047378541243623840, 0.8047378541243623840, 1.000000000000000000 ) ) 
 REPRESENTATION_ITEM ( '' )  );
#13925 =( NAMED_UNIT ( * ) SI_UNIT ( $, .STERADIAN. ) SOLID_ANGLE_UNIT ( ) );
#13926 = CLOSED_SHELL ( 'NONE', ( #4112, #2935, #5648, #17065, #10499, #17386, #6396, #3099, #4459, #8357, #3938, #20046, #14420, #11457, #8250, #11633, #7148, #6172, #3791, #12792, #18554, #10550, #9211, #14974, #3704, #6089, #15348, #13078, #16105, #13603, #4120, #14128, #8637, #18054, #5088, #16676, #6365, #3511, #14495, #4589, #11927, #9390, #17224, #16932 ) ) ;
#13927 = VERTEX_POINT ( 'NONE', #5578 ) ;
#13928 = AXIS2_PLACEMENT_3D ( 'NONE', #15144, #20063, #18732 ) ;
#13929 = CARTESIAN_POINT ( 'NONE',  ( -23.00000000000002132, 10.00000000000000000, 37.00000000000000711 ) ) ;
#13930 = CARTESIAN_POINT ( 'NONE',  ( 178.4893729001365728, 123.1299228374914918, 29.36128450348865471 ) ) ;
#13931 = EDGE_CURVE ( 'NONE', #305, #9522, #13817, .T. ) ;
#13932 = AXIS2_PLACEMENT_3D ( 'NONE', #11981, #19671, #7336 ) ;
#13933 = PRESENTATION_LAYER_ASSIGNMENT (  '', '', ( #8025 ) ) ;
#13934 = ORIENTED_EDGE ( 'NONE', *, *, #15060, .T. ) ;
#13935 =( LENGTH_UNIT ( ) NAMED_UNIT ( * ) SI_UNIT ( .MILLI., .METRE. ) );
#13936 = VERTEX_POINT ( 'NONE', #5800 ) ;
#13937 = AXIS2_PLACEMENT_3D ( 'NONE', #16986, #20144, #1068 ) ;
#13938 = EDGE_CURVE ( 'NONE', #13149, #17286, #10431, .T. ) ;
#13939 = FACE_OUTER_BOUND ( 'NONE', #12870, .T. ) ;
#13940 = LINE ( 'NONE', #11149, #8241 ) ;
#13941 = VERTEX_POINT ( 'NONE', #14973 ) ;
#13942 = PLANE ( 'NONE',  #5790 ) ;
#13943 = CARTESIAN_POINT ( 'NONE',  ( 109.4893729001366012, 129.7247684487574588, 368.0000000000000000 ) ) ;
#13944 = DIRECTION ( 'NONE',  ( 0.000000000000000000, 0.000000000000000000, 1.000000000000000000 ) ) ;
#13945 = ADVANCED_FACE ( 'NONE', ( #9090 ), #1212, .F. ) ;
#13946 = AXIS2_PLACEMENT_3D ( 'NONE', #13050, #17660, #5098 ) ;
#13947 = ADVANCED_FACE ( 'NONE', ( #18039 ), #10216, .T. ) ;
#13948 = STYLED_ITEM ( 'NONE', ( #5170 ), #7851 ) ;
#13949 = CARTESIAN_POINT ( 'NONE',  ( 53.48937290013660117, 77.72476844875745883, 250.0000000000000000 ) ) ;
#13950 = VECTOR ( 'NONE', #18144, 1000.000000000000000 ) ;
#13951 = ORIENTED_EDGE ( 'NONE', *, *, #12284, .F. ) ;
#13952 =( NAMED_UNIT ( * ) PLANE_ANGLE_UNIT ( ) SI_UNIT ( $, .RADIAN. ) );
#13953 = VERTEX_POINT ( 'NONE', #7151 ) ;
#13954 = CARTESIAN_POINT ( 'NONE',  ( 55.48937290013659407, 211.0574367717017594, 346.4752554294135507 ) ) ;
#13955 = LINE ( 'NONE', #3233, #2418 ) ;
#13956 = ITEM_DEFINED_TRANSFORMATION ( 'NONE', 'NONE', #19206,  #2741 ) ;
#13957 = PRESENTATION_LAYER_ASSIGNMENT (  '', '', ( #15269 ) ) ;
#13958 = ORIENTED_EDGE ( 'NONE', *, *, #6356, .F. ) ;
#13959 = ORIENTED_EDGE ( 'NONE', *, *, #11088, .F. ) ;
#13960 = CIRCLE ( 'NONE', #9024, 3.000000000000002665 ) ;
#13961 = LINE ( 'NONE', #7784, #2023 ) ;
#13962 = ORIENTED_EDGE ( 'NONE', *, *, #6739, .T. ) ;
#13963 = VECTOR ( 'NONE', #2625, 1000.000000000000000 ) ;
#13964 = ORIENTED_EDGE ( 'NONE', *, *, #15255, .T. ) ;
#13965 = VERTEX_POINT ( 'NONE', #2583 ) ;
#13966 = PRESENTATION_LAYER_ASSIGNMENT (  '', '', ( #8697 ) ) ;
#13967 = CIRCLE ( 'NONE', #8058, 10.00000000000001066 ) ;
#13968 = CIRCLE ( 'NONE', #471, 4.000000000000007105 ) ;
#13969 = DIRECTION ( 'NONE',  ( 1.000000000000000000, 0.000000000000000000, 0.000000000000000000 ) ) ;
#13970 = VECTOR ( 'NONE', #1745, 1000.000000000000000 ) ;
#13971 = ORIENTED_EDGE ( 'NONE', *, *, #15614, .T. ) ;
#13972 = CARTESIAN_POINT ( 'NONE',  ( 0.000000000000000000, 5.352861011586007481E-13, -75.00000000000599698 ) ) ;
#13973 = CARTESIAN_POINT ( 'NONE',  ( -26.00000000000000000, 19.00000000000000000, 40.00000000000001421 ) ) ;
#13974 = VECTOR ( 'NONE', #17496, 1000.000000000000000 ) ;
#13975 = EDGE_CURVE ( 'NONE', #17548, #13169, #4039, .T. ) ;
#13976 = AXIS2_PLACEMENT_3D ( 'NONE', #13273, #19520, #5441 ) ;
#13977 = CARTESIAN_POINT ( 'NONE',  ( 503.8334540492693918, 191.8198460455371333, 235.0057801310552463 ) ) ;
#13978 = MECHANICAL_DESIGN_GEOMETRIC_PRESENTATION_REPRESENTATION (  '', ( #18246 ), #5104 ) ;
#13979 = DIRECTION ( 'NONE',  ( 0.000000000000000000, 0.000000000000000000, -1.000000000000000000 ) ) ;
#13980 = SURFACE_SIDE_STYLE ('',( #2937 ) ) ;
#13981 = DIRECTION ( 'NONE',  ( -1.000000000000000000, -0.000000000000000000, -0.000000000000000000 ) ) ;
#13982 = AXIS2_PLACEMENT_3D ( 'NONE', #13549, #751, #12011 ) ;
#13983 = COLOUR_RGB ( '', 0.66274510, 0.83137255, 0.94901961) ;
#13984 = DIRECTION ( 'NONE',  ( 0.000000000000000000, 0.000000000000000000, -1.000000000000000000 ) ) ;
#13985 = CARTESIAN_POINT ( 'NONE',  ( -31.00000000000005329, 0.000000000000000000, -26.00000000000000355 ) ) ;
#13986 =( NAMED_UNIT ( * ) SI_UNIT ( $, .STERADIAN. ) SOLID_ANGLE_UNIT ( ) );
#13988 = COLOUR_RGB ( '', 0.09019608, 0.27058824, 0.51372549) ;
#13987 = LINE ( 'NONE', #7897, #20242 ) ;
#13989 = FACE_BOUND ( 'NONE', #10533, .T. ) ;
#13990 = CARTESIAN_POINT ( 'NONE',  ( -0.7691948703060754733, 138.9269458084811788, 489.3115405995010292 ) ) ;
#13991 =( NAMED_UNIT ( * ) SI_UNIT ( $, .STERADIAN. ) SOLID_ANGLE_UNIT ( ) );
#13992 = EDGE_LOOP ( 'NONE', ( #11289, #6375 ) ) ;
#13993 =( GEOMETRIC_REPRESENTATION_CONTEXT ( 3 ) GLOBAL_UNCERTAINTY_ASSIGNED_CONTEXT ( ( #6845 ) ) GLOBAL_UNIT_ASSIGNED_CONTEXT ( ( #7124, #2887, #9176 ) ) REPRESENTATION_CONTEXT ( 'NONE', 'WORKASPACE' ) );
#13994 = VECTOR ( 'NONE', #6155, 1000.000000000000000 ) ;
#13995 = ORIENTED_EDGE ( 'NONE', *, *, #11745, .T. ) ;
#13996 = EDGE_LOOP ( 'NONE', ( #2339, #2651, #743, #9180 ) ) ;
#13997 = STYLED_ITEM ( 'NONE', ( #11680 ), #13061 ) ;
#13998 = CARTESIAN_POINT ( 'NONE',  ( -39.99999999999999289, 11.00000000000000000, -26.00000000000000355 ) ) ;
#13999 = CIRCLE ( 'NONE', #19269, 5.000000000000000888 ) ;
#14000 = ORIENTED_EDGE ( 'NONE', *, *, #17159, .F. ) ;
#14001 = AXIS2_PLACEMENT_3D ( 'NONE', #18907, #9527, #1889 ) ;
#14002 = ADVANCED_FACE ( 'NONE', ( #2491 ), #9174, .F. ) ;
#14003 = SURFACE_SIDE_STYLE ('',( #4926 ) ) ;
#14004 = ORIENTED_EDGE ( 'NONE', *, *, #13171, .F. ) ;
#14005 = CARTESIAN_POINT ( 'NONE',  ( 1.224646799147347044E-16, 38.00000000000000711, -0.9999999999999956701 ) ) ;
#14006 = CYLINDRICAL_SURFACE ( 'NONE', #8775, 10.00000000000000888 ) ;
#14007 = DIRECTION ( 'NONE',  ( 0.000000000000000000, 0.000000000000000000, 1.000000000000000000 ) ) ;
#14008 = PLANE ( 'NONE',  #3214 ) ;
#14009 = AXIS2_PLACEMENT_3D ( 'NONE', #10370, #3887, #12285 ) ;
#14010 = DIRECTION ( 'NONE',  ( 1.000000000000000000, 5.889072920838430686E-16, -0.000000000000000000 ) ) ;
#14011 =( NAMED_UNIT ( * ) PLANE_ANGLE_UNIT ( ) SI_UNIT ( $, .RADIAN. ) );
#14012 = DIRECTION ( 'NONE',  ( 0.000000000000000000, 0.000000000000000000, -1.000000000000000000 ) ) ;
#14013 = LINE ( 'NONE', #17304, #15856 ) ;
#14014 = CYLINDRICAL_SURFACE ( 'NONE', #20082, 10.00000000000000888 ) ;
#14015 = EDGE_CURVE ( 'NONE', #6891, #10970, #1308, .T. ) ;
#14016 = EDGE_LOOP ( 'NONE', ( #6772, #297, #15881, #5294, #14067, #14909 ) ) ;
#14017 = ORIENTED_EDGE ( 'NONE', *, *, #9001, .T. ) ;
#14018 = EDGE_LOOP ( 'NONE', ( #17292, #1381 ) ) ;
#14019 = CIRCLE ( 'NONE', #7118, 1.000000000000000888 ) ;
#14020 = CARTESIAN_POINT ( 'NONE',  ( 98.48937290013660117, 80.91625508013694912, 250.0000000000000000 ) ) ;
#14021 = VERTEX_POINT ( 'NONE', #1527 ) ;
#14022 = ORIENTED_EDGE ( 'NONE', *, *, #6617, .T. ) ;
#14023 = EDGE_LOOP ( 'NONE', ( #15799, #12842, #18597, #10901 ) ) ;
#14024 = LINE ( 'NONE', #20292, #2811 ) ;
#14025 = AXIS2_PLACEMENT_3D ( 'NONE', #16355, #2085, #552 ) ;
#14026 = VERTEX_POINT ( 'NONE', #13920 ) ;
#14027 = DIRECTION ( 'NONE',  ( -0.000000000000000000, -0.000000000000000000, -1.000000000000000000 ) ) ;
#14028 =( NAMED_UNIT ( * ) PLANE_ANGLE_UNIT ( ) SI_UNIT ( $, .RADIAN. ) );
#14029 = DIRECTION ( 'NONE',  ( 1.000000000000000000, 0.000000000000000000, 0.000000000000000000 ) ) ;
#14030 = CARTESIAN_POINT ( 'NONE',  ( -1.000000000000011768, 141.3905724437643414, 503.0282008302663144 ) ) ;
#14031 = PRODUCT_DEFINITION_SHAPE ( 'NONE', 'NONE',  #5698 ) ;
#14032 = ORIENTED_EDGE ( 'NONE', *, *, #3039, .F. ) ;
#14033 = EDGE_CURVE ( 'NONE', #8120, #3236, #3102, .T. ) ;
#14034 = LINE ( 'NONE', #6307, #5377 ) ;
#14035 = FILL_AREA_STYLE ('',( #7942 ) ) ;
#14036 = STYLED_ITEM ( 'NONE', ( #2555 ), #2949 ) ;
#14037 = CARTESIAN_POINT ( 'NONE',  ( 0.000000000000000000, 216.7545334744432921, 495.1946179577816451 ) ) ;
#14038 = ADVANCED_FACE ( 'NONE', ( #1424 ), #14221, .F. ) ;
#14039 = EDGE_LOOP ( 'NONE', ( #15416, #4083, #4077, #17958 ) ) ;
#14040 = DIRECTION ( 'NONE',  ( 0.000000000000000000, 1.000000000000000000, 0.000000000000000000 ) ) ;
#14041 = SURFACE_STYLE_FILL_AREA ( #11050 ) ;
#14042 = ADVANCED_BREP_SHAPE_REPRESENTATION ( '', ( #1227, #2741 ), #14554 ) ;
#14043 = CARTESIAN_POINT ( 'NONE',  ( 0.000000000000000000, 16.00000000000000000, 0.000000000000000000 ) ) ;
#14044 = AXIS2_PLACEMENT_3D ( 'NONE', #5955, #18512, #10699 ) ;
#14045 = EDGE_CURVE ( 'NONE', #14156, #9509, #5708, .T. ) ;
#14046 = EDGE_LOOP ( 'NONE', ( #2752, #16699 ) ) ;
#14047 = EDGE_CURVE ( 'NONE', #17623, #10970, #5061, .T. ) ;
#14048 = ORIENTED_EDGE ( 'NONE', *, *, #17690, .F. ) ;
#14049 = SURFACE_STYLE_USAGE ( .BOTH. , #14136 ) ;
#14050 = AXIS2_PLACEMENT_3D ( 'NONE', #16382, #18082, #13090 ) ;
#14051 = EDGE_LOOP ( 'NONE', ( #15135, #3022, #2720, #11241 ) ) ;
#14053 = EDGE_CURVE ( 'NONE', #5220, #10613, #9392, .T. ) ;
#14052 = SURFACE_SIDE_STYLE ('',( #7772 ) ) ;
#14054 = CARTESIAN_POINT ( 'NONE',  ( 0.4336145047205204883, 139.5236339024991423, 500.3048018832922708 ) ) ;
#14055 = CARTESIAN_POINT ( 'NONE',  ( -26.00000000000002842, 0.000000000000000000, -39.99999999999999289 ) ) ;
#14056 = LINE ( 'NONE', #7964, #5109 ) ;
#14057 = LINE ( 'NONE', #12296, #18251 ) ;
#14058 = ORIENTED_EDGE ( 'NONE', *, *, #11891, .T. ) ;
#14059 = FACE_OUTER_BOUND ( 'NONE', #20362, .T. ) ;
#14060 = DIRECTION ( 'NONE',  ( 1.000000000000000000, 0.000000000000000000, -0.000000000000000000 ) ) ;
#14061 = DIRECTION ( 'NONE',  ( -0.000000000000000000, -1.000000000000000000, 0.000000000000000000 ) ) ;
#14062 = EDGE_CURVE ( 'NONE', #3302, #10482, #6713, .T. ) ;
#14063 = ORIENTED_EDGE ( 'NONE', *, *, #2864, .F. ) ;
#14064 = ORIENTED_EDGE ( 'NONE', *, *, #2016, .T. ) ;
#14065 = EDGE_CURVE ( 'NONE', #5026, #2094, #17324, .T. ) ;
#14066 = ORIENTED_EDGE ( 'NONE', *, *, #13145, .T. ) ;
#14067 = ORIENTED_EDGE ( 'NONE', *, *, #3078, .F. ) ;
#14068 = SURFACE_STYLE_USAGE ( .BOTH. , #246 ) ;
#14069 = ORIENTED_EDGE ( 'NONE', *, *, #6833, .F. ) ;
#14070 = DIRECTION ( 'NONE',  ( 6.123031769111888756E-17, 0.000000000000000000, 1.000000000000000000 ) ) ;
#14071 = ORIENTED_EDGE ( 'NONE', *, *, #9503, .T. ) ;
#14072 = CARTESIAN_POINT ( 'NONE',  ( -25.99999999999999645, 0.000000000000000000, -31.00000000000003197 ) ) ;
#14073 = CARTESIAN_POINT ( 'NONE',  ( -79.99999999999995737, 140.0803381460330002, 488.6808864560385359 ) ) ;
#14074 = CYLINDRICAL_SURFACE ( 'NONE', #5135, 18.50000000000000000 ) ;
#14075 = CARTESIAN_POINT ( 'NONE',  ( 0.000000000000000000, 341.0487089519837696, -133.5000000000032969 ) ) ;
#14076 = DIRECTION ( 'NONE',  ( 0.000000000000000000, 1.000000000000000000, 0.000000000000000000 ) ) ;
#14077 = ADVANCED_FACE ( 'NONE', ( #12480 ), #20089, .T. ) ;
#14078 = EDGE_LOOP ( 'NONE', ( #11892, #1179, #8726, #3431 ) ) ;
#14079 = FILL_AREA_STYLE ('',( #1483 ) ) ;
#14080 = PLANE ( 'NONE',  #5370 ) ;
#14081 = DIRECTION ( 'NONE',  ( 0.000000000000000000, 1.000000000000000000, 0.000000000000000000 ) ) ;
#14082 =( NAMED_UNIT ( * ) PLANE_ANGLE_UNIT ( ) SI_UNIT ( $, .RADIAN. ) );
#14083 = DIRECTION ( 'NONE',  ( 1.000000000000000000, 0.000000000000000000, 0.000000000000000000 ) ) ;
#14084 = CARTESIAN_POINT ( 'NONE',  ( 0.05802186526201238287, 138.7922706605886276, 490.2433561606925423 ) ) ;
#14085 = CARTESIAN_POINT ( 'NONE',  ( 0.000000000000000000, 341.0487089519837696, -115.0000000000032969 ) ) ;
#14086 = ADVANCED_FACE ( 'NONE', ( #5990 ), #7637, .F. ) ;
#14087 = ORIENTED_EDGE ( 'NONE', *, *, #16140, .F. ) ;
#14088 = VERTEX_POINT ( 'NONE', #12387 ) ;
#14089 = ORIENTED_EDGE ( 'NONE', *, *, #19336, .F. ) ;
#14090 = VERTEX_POINT ( 'NONE', #18657 ) ;
#14091 = DIRECTION ( 'NONE',  ( 3.295974604355930324E-14, 0.000000000000000000, -1.000000000000000000 ) ) ;
#14092 = PLANE ( 'NONE',  #6150 ) ;
#14093 = VERTEX_POINT ( 'NONE', #15701 ) ;
#14094 = CARTESIAN_POINT ( 'NONE',  ( 111.4893729001366012, 127.7247684487574588, 370.0000000000000000 ) ) ;
#14095 = ORIENTED_EDGE ( 'NONE', *, *, #13441, .F. ) ;
#14096 =( NAMED_UNIT ( * ) SI_UNIT ( $, .STERADIAN. ) SOLID_ANGLE_UNIT ( ) );
#14097 = DIRECTION ( 'NONE',  ( 1.000000000000000000, 0.000000000000000000, 0.000000000000000000 ) ) ;
#14098 = LINE ( 'NONE', #4317, #4136 ) ;
#14099 = CIRCLE ( 'NONE', #10808, 3.000000000000002665 ) ;
#14100 = DIRECTION ( 'NONE',  ( 0.000000000000000000, 0.000000000000000000, 1.000000000000000000 ) ) ;
#14101 = CARTESIAN_POINT ( 'NONE',  ( 78.48937290013660117, 123.1299228374914208, 220.6387154965113382 ) ) ;
#14102 = CARTESIAN_POINT ( 'NONE',  ( 36.00000000000000000, 0.000000000000000000, -135.0000000000000284 ) ) ;
#14103 = DIRECTION ( 'NONE',  ( 0.000000000000000000, 0.000000000000000000, -1.000000000000000000 ) ) ;
#14104 = DIRECTION ( 'NONE',  ( 0.000000000000000000, 1.000000000000000000, 0.000000000000000000 ) ) ;
#14105 =( NAMED_UNIT ( * ) SI_UNIT ( $, .STERADIAN. ) SOLID_ANGLE_UNIT ( ) );
#14106 = EDGE_CURVE ( 'NONE', #15780, #17589, #9482, .T. ) ;
#14107 = ORIENTED_EDGE ( 'NONE', *, *, #14596, .T. ) ;
#14108 = ORIENTED_EDGE ( 'NONE', *, *, #15682, .F. ) ;
#14109 = MECHANICAL_DESIGN_GEOMETRIC_PRESENTATION_REPRESENTATION (  '', ( #14125 ), #5856 ) ;
#14110 = ORIENTED_EDGE ( 'NONE', *, *, #10828, .F. ) ;
#14111 = EDGE_LOOP ( 'NONE', ( #3570, #14761, #5258, #12522 ) ) ;
#14112 = ORIENTED_EDGE ( 'NONE', *, *, #16621, .T. ) ;
#14113 = CARTESIAN_POINT ( 'NONE',  ( -23.00000000000002132, 6.000000000000000000, 32.00000000000000000 ) ) ;
#14114 = FILL_AREA_STYLE_COLOUR ( '', #2100 ) ;
#14115 = CARTESIAN_POINT ( 'NONE',  ( -15.00000000000000000, 317.7545334744432353, 495.1946179577816451 ) ) ;
#14116 = CYLINDRICAL_SURFACE ( 'NONE', #12062, 3.299999999999997158 ) ;
#14117 = SURFACE_SIDE_STYLE ('',( #1526 ) ) ;
#14118 = FILL_AREA_STYLE_COLOUR ( '', #13293 ) ;
#14119 = DIRECTION ( 'NONE',  ( 0.000000000000000000, -0.000000000000000000, 1.000000000000000000 ) ) ;
#14120 = FACE_BOUND ( 'NONE', #12947, .T. ) ;
#14121 = AXIS2_PLACEMENT_3D ( 'NONE', #701, #16795, #13500 ) ;
#14122 = DIRECTION ( 'NONE',  ( 0.000000000000000000, 0.000000000000000000, 1.000000000000000000 ) ) ;
#14123 = CARTESIAN_POINT ( 'NONE',  ( -4.848803763073570445E-15, 146.8256012863087108, 507.0490161104376057 ) ) ;
#14124 = EDGE_LOOP ( 'NONE', ( #10140, #844, #16769, #13139 ) ) ;
#14125 = STYLED_ITEM ( 'NONE', ( #2814 ), #11116 ) ;
#14126 = CARTESIAN_POINT ( 'NONE',  ( -79.99999999999995737, 216.7545334744432921, 515.1946179577817020 ) ) ;
#14127 = DIRECTION ( 'NONE',  ( 0.000000000000000000, 1.000000000000000000, 0.000000000000000000 ) ) ;
#14128 = ADVANCED_FACE ( 'NONE', ( #16208 ), #607, .T. ) ;
#14129 = ORIENTED_EDGE ( 'NONE', *, *, #7283, .T. ) ;
#14130 = AXIS2_PLACEMENT_3D ( 'NONE', #6171, #1692, #8005 ) ;
#14131 = VECTOR ( 'NONE', #8460, 1000.000000000000000 ) ;
#14132 = AXIS2_PLACEMENT_3D ( 'NONE', #8302, #1883, #11390 ) ;
#14133 = EDGE_CURVE ( 'NONE', #13107, #3178, #12970, .T. ) ;
#14134 = ORIENTED_EDGE ( 'NONE', *, *, #17852, .T. ) ;
#14135 = PLANE ( 'NONE',  #13014 ) ;
#14136 = SURFACE_SIDE_STYLE ('',( #17428 ) ) ;
#14137 = ORIENTED_EDGE ( 'NONE', *, *, #12347, .T. ) ;
#14138 = LINE ( 'NONE', #23, #1751 ) ;
#14139 =( NAMED_UNIT ( * ) PLANE_ANGLE_UNIT ( ) SI_UNIT ( $, .RADIAN. ) );
#14140 = CARTESIAN_POINT ( 'NONE',  ( 0.9999999999998814282, 140.4048636633015121, 500.8237260975781737 ) ) ;
#14141 = DIRECTION ( 'NONE',  ( 0.000000000000000000, -1.000000000000000000, 0.000000000000000000 ) ) ;
#14142 = DIRECTION ( 'NONE',  ( -0.000000000000000000, -1.000000000000000000, -0.000000000000000000 ) ) ;
#14143 = VERTEX_POINT ( 'NONE', #6506 ) ;
#14144 = DIRECTION ( 'NONE',  ( 0.000000000000000000, -0.9497703099767278445, -0.3129478523439812032 ) ) ;
#14145 = EDGE_CURVE ( 'NONE', #3589, #15013, #2073, .T. ) ;
#14146 =( NAMED_UNIT ( * ) SI_UNIT ( $, .STERADIAN. ) SOLID_ANGLE_UNIT ( ) );
#14147 = CONTEXT_DEPENDENT_SHAPE_REPRESENTATION ( #7114, #12732 ) ;
#14148 = CIRCLE ( 'NONE', #7252, 1.000000000000000444 ) ;
#14149 = AXIS2_PLACEMENT_3D ( 'NONE', #10142, #16442, #8583 ) ;
#14150 = ORIENTED_EDGE ( 'NONE', *, *, #574, .T. ) ;
#14151 = EDGE_LOOP ( 'NONE', ( #9422, #8193, #14796, #18028 ) ) ;
#14152 = CARTESIAN_POINT ( 'NONE',  ( 153.4893729001366864, 113.1299228374914634, 79.58252780074349175 ) ) ;
#14153 = ORIENTED_EDGE ( 'NONE', *, *, #11025, .F. ) ;
#14154 = ORIENTED_EDGE ( 'NONE', *, *, #11382, .F. ) ;
#14155 = EDGE_CURVE ( 'NONE', #3606, #7437, #3824, .T. ) ;
#14156 = VERTEX_POINT ( 'NONE', #9897 ) ;
#14157 = LINE ( 'NONE', #4892, #14676 ) ;
#14158 = EDGE_CURVE ( 'NONE', #14439, #18534, #13209, .T. ) ;
#14159 = ORIENTED_EDGE ( 'NONE', *, *, #19079, .F. ) ;
#14160 = DIRECTION ( 'NONE',  ( -1.000000000000000000, 0.000000000000000000, 0.000000000000000000 ) ) ;
#14161 = VECTOR ( 'NONE', #16614, 1000.000000000000000 ) ;
#14162 = ORIENTED_EDGE ( 'NONE', *, *, #843, .F. ) ;
#14163 = EDGE_CURVE ( 'NONE', #12468, #14259, #233, .T. ) ;
#14164 = CARTESIAN_POINT ( 'NONE',  ( -1.019150042136374168E-14, 152.4824555358011082, 486.3411705753778165 ) ) ;
#14165 = CIRCLE ( 'NONE', #11543, 1.000000000000000888 ) ;
#14166 = DIRECTION ( 'NONE',  ( 0.000000000000000000, 1.224646799147356165E-16, 1.000000000000000000 ) ) ;
#14167 = DIRECTION ( 'NONE',  ( 0.000000000000000000, -1.000000000000000000, 0.000000000000000000 ) ) ;
#14168 = CARTESIAN_POINT ( 'NONE',  ( -79.99999999999995737, 138.7545334744432637, 510.3921618609452935 ) ) ;
#14169 = ADVANCED_FACE ( 'NONE', ( #6828, #19455, #398, #2242, #8160 ), #3617, .F. ) ;
#14170 = DIRECTION ( 'NONE',  ( 0.000000000000000000, -0.000000000000000000, 1.000000000000000000 ) ) ;
#14171 =( NAMED_UNIT ( * ) PLANE_ANGLE_UNIT ( ) SI_UNIT ( $, .RADIAN. ) );
#14172 = LINE ( 'NONE', #11491, #6750 ) ;
#14173 = CIRCLE ( 'NONE', #13212, 2.000000000000001776 ) ;
#14174 = ORIENTED_EDGE ( 'NONE', *, *, #16245, .F. ) ;
#14175 = EDGE_CURVE ( 'NONE', #5141, #16598, #15262, .T. ) ;
#14176 = CARTESIAN_POINT ( 'NONE',  ( 0.000000000000000000, 309.2289037985890445, -146.8198051533984199 ) ) ;
#14177 = DIRECTION ( 'NONE',  ( 0.000000000000000000, 0.000000000000000000, -1.000000000000000000 ) ) ;
#14178 =( NAMED_UNIT ( * ) SI_UNIT ( $, .STERADIAN. ) SOLID_ANGLE_UNIT ( ) );
#14179 = DIRECTION ( 'NONE',  ( 0.000000000000000000, 0.000000000000000000, -1.000000000000000000 ) ) ;
#14180 = CARTESIAN_POINT ( 'NONE',  ( 1.050000000000000044, -17.52499999999999858, -2.146193515505736390E-15 ) ) ;
#14181 = DIRECTION ( 'NONE',  ( -7.557006526585458208E-17, 0.7699350945217602327, 0.6381222063396385646 ) ) ;
#14182 = SURFACE_STYLE_FILL_AREA ( #4915 ) ;
#14183 = ORIENTED_EDGE ( 'NONE', *, *, #6780, .F. ) ;
#14184 = CIRCLE ( 'NONE', #1303, 15.14120580695350071 ) ;
#14185 =( GEOMETRIC_REPRESENTATION_CONTEXT ( 3 ) GLOBAL_UNCERTAINTY_ASSIGNED_CONTEXT ( ( #16748 ) ) GLOBAL_UNIT_ASSIGNED_CONTEXT ( ( #15242, #1185, #18899 ) ) REPRESENTATION_CONTEXT ( 'NONE', 'WORKASPACE' ) );
#14186 = EDGE_LOOP ( 'NONE', ( #2726, #15804, #10156, #4764 ) ) ;
#14187 = ORIENTED_EDGE ( 'NONE', *, *, #10228, .F. ) ;
#14188 = CARTESIAN_POINT ( 'NONE',  ( -82.18192946989245229, 147.7545334744432921, 491.0690926367355473 ) ) ;
#14189 = CARTESIAN_POINT ( 'NONE',  ( -78.99999999999995737, 140.8764026050587290, 502.4686618848273270 ) ) ;
#14190 = ORIENTED_EDGE ( 'NONE', *, *, #16715, .F. ) ;
#14191 = DIRECTION ( 'NONE',  ( 0.000000000000000000, 0.000000000000000000, -1.000000000000000000 ) ) ;
#14192 = ORIENTED_EDGE ( 'NONE', *, *, #16329, .F. ) ;
#14193 = EDGE_CURVE ( 'NONE', #7139, #17623, #15537, .T. ) ;
#14194 = COLOUR_RGB ( '', 0.08235294, 0.09019608, 0.10196078) ;
#14195 = FILL_AREA_STYLE_COLOUR ( '', #19463 ) ;
#14196 = FACE_BOUND ( 'NONE', #3924, .T. ) ;
#14197 = EDGE_CURVE ( 'NONE', #10884, #16969, #13311, .T. ) ;
#14198 = CARTESIAN_POINT ( 'NONE',  ( -0.9714722756524757363, 62.84506667638981270, 9.451944983354374941 ) ) ;
#14199 = CIRCLE ( 'NONE', #10256, 8.000000000000000000 ) ;
#14200 = LINE ( 'NONE', #12774, #15404 ) ;
#14201 = EDGE_CURVE ( 'NONE', #5831, #19951, #6369, .T. ) ;
#14202 = FACE_OUTER_BOUND ( 'NONE', #11700, .T. ) ;
#14203 = DIRECTION ( 'NONE',  ( 0.000000000000000000, 0.000000000000000000, 1.000000000000000000 ) ) ;
#14204 = DIRECTION ( 'NONE',  ( -0.000000000000000000, -0.000000000000000000, 1.000000000000000000 ) ) ;
#14205 = DIRECTION ( 'NONE',  ( 0.000000000000000000, -0.000000000000000000, 1.000000000000000000 ) ) ;
#14206 = DIRECTION ( 'NONE',  ( 1.000000000000000000, 0.000000000000000000, 0.000000000000000000 ) ) ;
#14207 = CARTESIAN_POINT ( 'NONE',  ( -20.99999999999999645, 19.00000000000000000, 35.00000000000001421 ) ) ;
#14208 = ORIENTED_EDGE ( 'NONE', *, *, #5076, .F. ) ;
#14209 = VECTOR ( 'NONE', #16069, 1000.000000000000000 ) ;
#14210 = ORIENTED_EDGE ( 'NONE', *, *, #15864, .T. ) ;
#14211 = LINE ( 'NONE', #12570, #6425 ) ;
#14212 = CIRCLE ( 'NONE', #12226, 3.283624802691453848 ) ;
#14213 = ORIENTED_EDGE ( 'NONE', *, *, #10869, .T. ) ;
#14214 = ORIENTED_EDGE ( 'NONE', *, *, #5207, .T. ) ;
#14215 = ORIENTED_EDGE ( 'NONE', *, *, #17549, .T. ) ;
#14216 = CARTESIAN_POINT ( 'NONE',  ( -15.00000000000000000, 316.7545334744432353, 475.1454018718993098 ) ) ;
#14217 = FACE_OUTER_BOUND ( 'NONE', #20126, .T. ) ;
#14218 = CARTESIAN_POINT ( 'NONE',  ( 1.050000000000000044, 0.000000000000000000, 0.000000000000000000 ) ) ;
#14219 = DIRECTION ( 'NONE',  ( 0.000000000000000000, 0.000000000000000000, -1.000000000000000000 ) ) ;
#14220 = EDGE_CURVE ( 'NONE', #17973, #16787, #7020, .T. ) ;
#14221 = CYLINDRICAL_SURFACE ( 'NONE', #8354, 17.52499999999999858 ) ;
#14222 = PRESENTATION_STYLE_ASSIGNMENT (( #1850 ) ) ;
#14223 = AXIS2_PLACEMENT_3D ( 'NONE', #9978, #380, #11621 ) ;
#14224 = AXIS2_PLACEMENT_3D ( 'NONE', #20239, #18886, #3237 ) ;
#14225 = SURFACE_STYLE_USAGE ( .BOTH. , #17412 ) ;
#14226 = LINE ( 'NONE', #4959, #5692 ) ;
#14227 = DIRECTION ( 'NONE',  ( -0.000000000000000000, -0.000000000000000000, 1.000000000000000000 ) ) ;
#14228 = ORIENTED_EDGE ( 'NONE', *, *, #443, .F. ) ;
#14229 = CARTESIAN_POINT ( 'NONE',  ( -79.99999999999995737, 142.0976792249509231, 485.4122383872432351 ) ) ;
#14230 = CARTESIAN_POINT ( 'NONE',  ( -21.85283368562565443, 317.7545334744432353, 489.0536462814662855 ) ) ;
#14231 = PRODUCT_DEFINITION_FORMATION_WITH_SPECIFIED_SOURCE ( 'ANY', '', #5172, .NOT_KNOWN. ) ;
#14232 = STYLED_ITEM ( 'NONE', ( #15536 ), #3321 ) ;
#14233 = VECTOR ( 'NONE', #2687, 1000.000000000000000 ) ;
#14234 = EDGE_LOOP ( 'NONE', ( #17251, #12104, #4333, #3538 ) ) ;
#14235 = AXIS2_PLACEMENT_3D ( 'NONE', #6167, #57, #3166 ) ;
#14236 = AXIS2_PLACEMENT_3D ( 'NONE', #18913, #11187, #15850 ) ;
#14237 = DIRECTION ( 'NONE',  ( 1.000000000000000000, 0.000000000000000000, 0.000000000000000000 ) ) ;
#14238 = MECHANICAL_DESIGN_GEOMETRIC_PRESENTATION_REPRESENTATION (  '', ( #8974 ), #3036 ) ;
#14239 = ORIENTED_EDGE ( 'NONE', *, *, #978, .F. ) ;
#14240 = LINE ( 'NONE', #12499, #1442 ) ;
#14241 = CARTESIAN_POINT ( 'NONE',  ( 25.99999999999996092, 3.000000000000000000, 40.00000000000000711 ) ) ;
#14242 = VERTEX_POINT ( 'NONE', #18611 ) ;
#14243 = LINE ( 'NONE', #17430, #18932 ) ;
#14244 = FACE_OUTER_BOUND ( 'NONE', #4905, .T. ) ;
#14245 = CARTESIAN_POINT ( 'NONE',  ( 0.000000000000000000, -5.000000000000000888, -150.0000000000000000 ) ) ;
#14246 = CARTESIAN_POINT ( 'NONE',  ( 0.9999999999998516742, 139.7462607836631605, 500.8237260975782874 ) ) ;
#14247 = CARTESIAN_POINT ( 'NONE',  ( -1.561251128379126385E-14, 147.7545334744432921, 491.0690926367356042 ) ) ;
#14248 = CARTESIAN_POINT ( 'NONE',  ( 503.8334540492693918, 191.8198460455371333, 168.2339398819845826 ) ) ;
#14249 = ORIENTED_EDGE ( 'NONE', *, *, #11630, .F. ) ;
#14250 = SURFACE_STYLE_USAGE ( .BOTH. , #3015 ) ;
#14251 = VECTOR ( 'NONE', #2932, 1000.000000000000000 ) ;
#14252 = CIRCLE ( 'NONE', #12269, 3.000000000000016431 ) ;
#14253 = CONTEXT_DEPENDENT_SHAPE_REPRESENTATION ( #8434, #11228 ) ;
#14254 = ORIENTED_EDGE ( 'NONE', *, *, #15018, .T. ) ;
#14255 = PRODUCT_DEFINITION ( 'UNKNOWN', '', #9972, #796 ) ;
#14256 = ORIENTED_EDGE ( 'NONE', *, *, #5348, .F. ) ;
#14257 = ORIENTED_EDGE ( 'NONE', *, *, #13676, .T. ) ;
#14258 =( GEOMETRIC_REPRESENTATION_CONTEXT ( 3 ) GLOBAL_UNCERTAINTY_ASSIGNED_CONTEXT ( ( #10483 ) ) GLOBAL_UNIT_ASSIGNED_CONTEXT ( ( #15679, #1913, #9666 ) ) REPRESENTATION_CONTEXT ( 'NONE', 'WORKASPACE' ) );
#14259 = VERTEX_POINT ( 'NONE', #4500 ) ;
#14260 = EDGE_CURVE ( 'NONE', #10947, #10177, #2354, .T. ) ;
#14261 =( NAMED_UNIT ( * ) SI_UNIT ( $, .STERADIAN. ) SOLID_ANGLE_UNIT ( ) );
#14262 = VERTEX_POINT ( 'NONE', #9226 ) ;
#14263 = AXIS2_PLACEMENT_3D ( 'NONE', #4725, #11016, #6186 ) ;
#14264 = CIRCLE ( 'NONE', #16915, 4.000000000000000000 ) ;
#14265 = ORIENTED_EDGE ( 'NONE', *, *, #18731, .F. ) ;
#14266 = VECTOR ( 'NONE', #9153, 1000.000000000000000 ) ;
#14267 = CYLINDRICAL_SURFACE ( 'NONE', #4076, 10.00000000000001066 ) ;
#14268 = DIRECTION ( 'NONE',  ( -0.000000000000000000, -1.000000000000000000, -0.000000000000000000 ) ) ;
#14269 = DIRECTION ( 'NONE',  ( -0.000000000000000000, -1.000000000000000000, -0.000000000000000000 ) ) ;
#14270 = DIRECTION ( 'NONE',  ( 0.000000000000000000, 1.000000000000000000, 0.000000000000000000 ) ) ;
#14271 = COLOUR_RGB ( '', 0.72549020, 0.75294118, 0.79215686) ;
#14272 = EDGE_CURVE ( 'NONE', #3837, #11175, #5382, .T. ) ;
#14273 = CARTESIAN_POINT ( 'NONE',  ( -22.99999999999999645, 68.00000000000000000, 37.00000000000002132 ) ) ;
#14274 = VECTOR ( 'NONE', #393, 1000.000000000000000 ) ;
#14275 = ORIENTED_EDGE ( 'NONE', *, *, #17852, .F. ) ;
#14276 = CARTESIAN_POINT ( 'NONE',  ( 37.00000000000003553, -20.00000000000000000, 23.00000000000000355 ) ) ;
#14277 = FACE_OUTER_BOUND ( 'NONE', #16463, .T. ) ;
#14278 = CYLINDRICAL_SURFACE ( 'NONE', #5679, 9.000000000000007105 ) ;
#14279 = LINE ( 'NONE', #19002, #18859 ) ;
#14280 = FACE_BOUND ( 'NONE', #18083, .T. ) ;
#14281 = LINE ( 'NONE', #166, #16256 ) ;
#14282 = EDGE_CURVE ( 'NONE', #3192, #15503, #18020, .T. ) ;
#14283 = DIRECTION ( 'NONE',  ( 1.322943490866811299E-12, 0.000000000000000000, 1.000000000000000000 ) ) ;
#14284 = FACE_OUTER_BOUND ( 'NONE', #442, .T. ) ;
#14285 = ADVANCED_BREP_SHAPE_REPRESENTATION ( '', ( #15739, #2741 ), #14258 ) ;
#14286 = ORIENTED_EDGE ( 'NONE', *, *, #17332, .T. ) ;
#14287 =( GEOMETRIC_REPRESENTATION_CONTEXT ( 3 ) GLOBAL_UNCERTAINTY_ASSIGNED_CONTEXT ( ( #7446 ) ) GLOBAL_UNIT_ASSIGNED_CONTEXT ( ( #19994, #8984, #7462 ) ) REPRESENTATION_CONTEXT ( 'NONE', 'WORKASPACE' ) );
#14288 = AXIS2_PLACEMENT_3D ( 'NONE', #17044, #18580, #18277 ) ;
#14289 = EDGE_CURVE ( 'NONE', #16423, #19149, #17157, .T. ) ;
#14290 = AXIS2_PLACEMENT_3D ( 'NONE', #2893, #13530, #4555 ) ;
#14291 = ORIENTED_EDGE ( 'NONE', *, *, #12574, .T. ) ;
#14292 = ADVANCED_FACE ( 'NONE', ( #6159 ), #11757, .T. ) ;
#14293 = VECTOR ( 'NONE', #10289, 1000.000000000000000 ) ;
#14294 = ORIENTED_EDGE ( 'NONE', *, *, #19660, .T. ) ;
#14295 = FILL_AREA_STYLE ('',( #18629 ) ) ;
#14296 = EDGE_CURVE ( 'NONE', #2872, #13802, #167, .T. ) ;
#14297 = DIRECTION ( 'NONE',  ( -1.000000000000000000, 0.000000000000000000, 0.000000000000000000 ) ) ;
#14298 = ORIENTED_EDGE ( 'NONE', *, *, #9602, .F. ) ;
#14299 =( NAMED_UNIT ( * ) SI_UNIT ( $, .STERADIAN. ) SOLID_ANGLE_UNIT ( ) );
#14300 = ORIENTED_EDGE ( 'NONE', *, *, #3445, .T. ) ;
#14301 = STYLED_ITEM ( 'NONE', ( #9183 ), #19322 ) ;
#14302 = DIRECTION ( 'NONE',  ( -1.000000000000000000, 0.000000000000000000, 0.000000000000000000 ) ) ;
#14303 = VECTOR ( 'NONE', #9485, 1000.000000000000000 ) ;
#14304 = FACE_OUTER_BOUND ( 'NONE', #20313, .T. ) ;
#14305 =( NAMED_UNIT ( * ) SI_UNIT ( $, .STERADIAN. ) SOLID_ANGLE_UNIT ( ) );
#14306 =( GEOMETRIC_REPRESENTATION_CONTEXT ( 3 ) GLOBAL_UNCERTAINTY_ASSIGNED_CONTEXT ( ( #616 ) ) GLOBAL_UNIT_ASSIGNED_CONTEXT ( ( #11139, #15709, #19167 ) ) REPRESENTATION_CONTEXT ( 'NONE', 'WORKASPACE' ) );
#14307 = EDGE_CURVE ( 'NONE', #6883, #5981, #8406, .T. ) ;
#14308 = CARTESIAN_POINT ( 'NONE',  ( -64.99999999999995737, 317.7545334744432353, 475.1454018718993098 ) ) ;
#14309 = CARTESIAN_POINT ( 'NONE',  ( -21.85283368562565443, 319.7545334744432353, 489.0536462814662855 ) ) ;
#14310 = DIRECTION ( 'NONE',  ( 0.000000000000000000, 0.000000000000000000, 1.000000000000000000 ) ) ;
#14311 = LINE ( 'NONE', #7615, #14 ) ;
#14312 = LINE ( 'NONE', #17303, #18492 ) ;
#14313 = AXIS2_PLACEMENT_3D ( 'NONE', #16698, #19845, #5762 ) ;
#14314 = EDGE_LOOP ( 'NONE', ( #10795, #15443, #16702, #15981 ) ) ;
#14315 = CIRCLE ( 'NONE', #13013, 10.00000000000000888 ) ;
#14316 = DIRECTION ( 'NONE',  ( 0.000000000000000000, 0.000000000000000000, -1.000000000000000000 ) ) ;
#14317 = VECTOR ( 'NONE', #20167, 1000.000000000000000 ) ;
#14318 = EDGE_CURVE ( 'NONE', #15933, #13085, #18601, .T. ) ;
#14319 = ORIENTED_EDGE ( 'NONE', *, *, #2038, .T. ) ;
#14320 = STYLED_ITEM ( 'NONE', ( #17656 ), #12909 ) ;
#14321 =( GEOMETRIC_REPRESENTATION_CONTEXT ( 3 ) GLOBAL_UNCERTAINTY_ASSIGNED_CONTEXT ( ( #16327 ) ) GLOBAL_UNIT_ASSIGNED_CONTEXT ( ( #17609, #16089, #14506 ) ) REPRESENTATION_CONTEXT ( 'NONE', 'WORKASPACE' ) );
#14322 = EDGE_CURVE ( 'NONE', #7143, #9862, #19560, .T. ) ;
#14323 = ORIENTED_EDGE ( 'NONE', *, *, #6448, .F. ) ;
#14324 = UNCERTAINTY_MEASURE_WITH_UNIT (LENGTH_MEASURE( 1.000000000000000082E-05 ), #19246, 'distance_accuracy_value', 'NONE');
#14325 = AXIS2_PLACEMENT_3D ( 'NONE', #20344, #4810, #14270 ) ;
#14326 =( NAMED_UNIT ( * ) SI_UNIT ( $, .STERADIAN. ) SOLID_ANGLE_UNIT ( ) );
#14327 = EDGE_LOOP ( 'NONE', ( #4479, #14592 ) ) ;
#14328 = ORIENTED_EDGE ( 'NONE', *, *, #2501, .F. ) ;
#14329 = CARTESIAN_POINT ( 'NONE',  ( -78.99999999999995737, 147.7545334744432921, 496.6642397995874489 ) ) ;
#14330 = AXIS2_PLACEMENT_3D ( 'NONE', #10227, #2386, #8690 ) ;
#14331 = FILL_AREA_STYLE ('',( #14114 ) ) ;
#14332 = DIRECTION ( 'NONE',  ( 0.000000000000000000, 1.000000000000000000, 0.000000000000000000 ) ) ;
#14333 = DIRECTION ( 'NONE',  ( 0.000000000000000000, 0.000000000000000000, -1.000000000000000000 ) ) ;
#14334 = AXIS2_PLACEMENT_3D ( 'NONE', #9738, #19093, #12427 ) ;
#14335 = DIRECTION ( 'NONE',  ( -0.000000000000000000, -1.000000000000000000, -0.000000000000000000 ) ) ;
#14336 = CARTESIAN_POINT ( 'NONE',  ( 19.99999999999995381, 3.000000000000000000, -36.99999999999999289 ) ) ;
#14337 = FACE_OUTER_BOUND ( 'NONE', #13996, .T. ) ;
#14338 = DIRECTION ( 'NONE',  ( 1.000000000000000000, 0.000000000000000000, 0.000000000000000000 ) ) ;
#14339 = DIRECTION ( 'NONE',  ( -6.263247009234064878E-17, 0.6381222063396385646, -0.7699350945217602327 ) ) ;
#14340 = CARTESIAN_POINT ( 'NONE',  ( -21.85283368562565443, 319.7545334744432353, 481.2863735482146694 ) ) ;
#14341 = ORIENTED_EDGE ( 'NONE', *, *, #11288, .T. ) ;
#14342 = EDGE_CURVE ( 'NONE', #2874, #11813, #9059, .T. ) ;
#14343 = CARTESIAN_POINT ( 'NONE',  ( 178.4893729001365443, 0.000000000000000000, 250.0000000000000000 ) ) ;
#14344 = CARTESIAN_POINT ( 'NONE',  ( -79.99999999999995737, 0.000000000000000000, 205.1946179577815883 ) ) ;
#14345 = AXIS2_PLACEMENT_3D ( 'NONE', #16946, #20111, #6011 ) ;
#14346 = AXIS2_PLACEMENT_3D ( 'NONE', #19491, #16814, #2575 ) ;
#14347 = VERTEX_POINT ( 'NONE', #13414 ) ;
#14348 = ORIENTED_EDGE ( 'NONE', *, *, #4456, .F. ) ;
#14349 = CARTESIAN_POINT ( 'NONE',  ( 5.044974746830580337, 0.000000000000000000, 0.000000000000000000 ) ) ;
#14350 = ORIENTED_EDGE ( 'NONE', *, *, #3858, .T. ) ;
#14351 = CYLINDRICAL_SURFACE ( 'NONE', #4116, 12.00000000000000178 ) ;
#14352 = CARTESIAN_POINT ( 'NONE',  ( -23.00000000000002132, 0.000000000000000000, 37.00000000000000711 ) ) ;
#14353 = EDGE_LOOP ( 'NONE', ( #10369, #18052, #18944, #12968 ) ) ;
#14354 = FACE_OUTER_BOUND ( 'NONE', #1982, .T. ) ;
#14355 = VECTOR ( 'NONE', #12796, 1000.000000000000000 ) ;
#14356 = VECTOR ( 'NONE', #5058, 1000.000000000000000 ) ;
#14357 = CARTESIAN_POINT ( 'NONE',  ( 498.8117674897343932, 214.2156642432025251, 250.0000000000000000 ) ) ;
#14358 = DIRECTION ( 'NONE',  ( -1.000000000000000000, -0.000000000000000000, -0.000000000000000000 ) ) ;
#14359 = CARTESIAN_POINT ( 'NONE',  ( 25.99999999999996092, 3.000000000000000000, -31.00000000000003197 ) ) ;
#14360 =( NAMED_UNIT ( * ) PLANE_ANGLE_UNIT ( ) SI_UNIT ( $, .RADIAN. ) );
#14361 = ORIENTED_EDGE ( 'NONE', *, *, #17321, .T. ) ;
#14362 = LINE ( 'NONE', #18683, #6548 ) ;
#14363 = CARTESIAN_POINT ( 'NONE',  ( 22.99999999999999289, 0.000000000000000000, 37.00000000000002132 ) ) ;
#14364 = DIRECTION ( 'NONE',  ( -1.000000000000000000, -0.000000000000000000, 3.854941057726247958E-16 ) ) ;
#14365 = ITEM_DEFINED_TRANSFORMATION ( 'NONE', 'NONE', #16544,  #2741 ) ;
#14366 = PRODUCT_DEFINITION_SHAPE ( 'NONE', 'NONE',  #20377 ) ;
#14367 = ORIENTED_EDGE ( 'NONE', *, *, #9487, .T. ) ;
#14368 = PLANE ( 'NONE',  #20125 ) ;
#14369 = ORIENTED_EDGE ( 'NONE', *, *, #16196, .T. ) ;
#14370 = ORIENTED_EDGE ( 'NONE', *, *, #6887, .F. ) ;
#14371 = EDGE_CURVE ( 'NONE', #16025, #19038, #19650, .T. ) ;
#14372 = ORIENTED_EDGE ( 'NONE', *, *, #19971, .T. ) ;
#14373 = CIRCLE ( 'NONE', #17669, 4.999999999999997335 ) ;
#14374 = CARTESIAN_POINT ( 'NONE',  ( 53.48937290013659407, 145.9162550801369491, -97.94896630388704750 ) ) ;
#14375 = PRESENTATION_STYLE_ASSIGNMENT (( #12838 ) ) ;
#14376 = VERTEX_POINT ( 'NONE', #11855 ) ;
#14377 = CARTESIAN_POINT ( 'NONE',  ( 10.00000000000000000, 309.2289037985890445, -146.8198051533984199 ) ) ;
#14378 = FILL_AREA_STYLE_COLOUR ( '', #7922 ) ;
#14379 = DIRECTION ( 'NONE',  ( -0.000000000000000000, -1.000000000000000000, 0.000000000000000000 ) ) ;
#14380 =( NAMED_UNIT ( * ) SI_UNIT ( $, .STERADIAN. ) SOLID_ANGLE_UNIT ( ) );
#14381 = FILL_AREA_STYLE_COLOUR ( '', #1970 ) ;
#14382 = DIRECTION ( 'NONE',  ( 0.000000000000000000, 1.000000000000000000, 0.000000000000000000 ) ) ;
#14383 = ORIENTED_EDGE ( 'NONE', *, *, #9890, .F. ) ;
#14384 = DIRECTION ( 'NONE',  ( 0.000000000000000000, 0.000000000000000000, 1.000000000000000000 ) ) ;
#14385 = ADVANCED_FACE ( 'NONE', ( #9132 ), #15426, .F. ) ;
#14386 = FACE_OUTER_BOUND ( 'NONE', #16336, .T. ) ;
#14387 = CARTESIAN_POINT ( 'NONE',  ( 0.000000000000000000, 376.0487089519832011, -80.00000000000332534 ) ) ;
#14388 = DIRECTION ( 'NONE',  ( 0.000000000000000000, 0.000000000000000000, -1.000000000000000000 ) ) ;
#14389 =( NAMED_UNIT ( * ) SI_UNIT ( $, .STERADIAN. ) SOLID_ANGLE_UNIT ( ) );
#14390 =( NAMED_UNIT ( * ) PLANE_ANGLE_UNIT ( ) SI_UNIT ( $, .RADIAN. ) );
#14391 = ORIENTED_EDGE ( 'NONE', *, *, #20307, .F. ) ;
#14392 = EDGE_LOOP ( 'NONE', ( #5862, #19946, #3512, #18718 ) ) ;
#14393 = EDGE_CURVE ( 'NONE', #5490, #5074, #17620, .T. ) ;
#14394 =( GEOMETRIC_REPRESENTATION_CONTEXT ( 3 ) GLOBAL_UNCERTAINTY_ASSIGNED_CONTEXT ( ( #2087 ) ) GLOBAL_UNIT_ASSIGNED_CONTEXT ( ( #20169, #12364, #7821 ) ) REPRESENTATION_CONTEXT ( 'NONE', 'WORKASPACE' ) );
#14395 = ORIENTED_EDGE ( 'NONE', *, *, #5252, .F. ) ;
#14396 = LINE ( 'NONE', #11414, #10930 ) ;
#14397 = LINE ( 'NONE', #9548, #7790 ) ;
#14398 = ORIENTED_EDGE ( 'NONE', *, *, #16934, .T. ) ;
#14399 = DIRECTION ( 'NONE',  ( -0.000000000000000000, -1.000000000000000000, -0.000000000000000000 ) ) ;
#14400 = LINE ( 'NONE', #10802, #8955 ) ;
#14401 = EDGE_CURVE ( 'NONE', #7933, #11794, #51, .T. ) ;
#14402 = VERTEX_POINT ( 'NONE', #5010 ) ;
#14403 = CARTESIAN_POINT ( 'NONE',  ( 109.4893729001365870, 209.7811923590224978, 348.0151256184570343 ) ) ;
#14404 = FILL_AREA_STYLE_COLOUR ( '', #501 ) ;
#14405 = DIRECTION ( 'NONE',  ( 8.027491443112700323E-16, 0.7071067811865504593, -0.7071067811865445751 ) ) ;
#14406 = CARTESIAN_POINT ( 'NONE',  ( 503.8334540492693918, 191.8198460455371333, 91.76606011801541740 ) ) ;
#14407 = VECTOR ( 'NONE', #9597, 1000.000000000000000 ) ;
#14408 = PLANE ( 'NONE',  #11964 ) ;
#14409 = DIRECTION ( 'NONE',  ( -9.815121534730717399E-17, 1.000000000000000000, -2.352167425053297897E-16 ) ) ;
#14410 = ADVANCED_FACE ( 'NONE', ( #6355 ), #1678, .T. ) ;
#14411 = LINE ( 'NONE', #14508, #19808 ) ;
#14412 = CARTESIAN_POINT ( 'NONE',  ( -26.00000000000002132, 8.000000000000000000, 40.00000000000000711 ) ) ;
#14413 = VECTOR ( 'NONE', #878, 1000.000000000000000 ) ;
#14414 = DIRECTION ( 'NONE',  ( 1.000000000000000000, 0.000000000000000000, 0.000000000000000000 ) ) ;
#14415 = PLANE ( 'NONE',  #10181 ) ;
#14416 = EDGE_CURVE ( 'NONE', #3148, #20355, #17566, .T. ) ;
#14417 = ORIENTED_EDGE ( 'NONE', *, *, #1503, .T. ) ;
#14418 = VERTEX_POINT ( 'NONE', #16060 ) ;
#14419 = VERTEX_POINT ( 'NONE', #6557 ) ;
#14420 = ADVANCED_FACE ( 'NONE', ( #1479 ), #17368, .F. ) ;
#14421 = ORIENTED_EDGE ( 'NONE', *, *, #19351, .T. ) ;
#14422 = ORIENTED_EDGE ( 'NONE', *, *, #11842, .T. ) ;
#14423 = ORIENTED_EDGE ( 'NONE', *, *, #13338, .F. ) ;
#14424 = DIRECTION ( 'NONE',  ( -1.000000000000000000, 0.000000000000000000, 0.000000000000000000 ) ) ;
#14425 = CIRCLE ( 'NONE', #5544, 8.000000000000007105 ) ;
#14426 = DIRECTION ( 'NONE',  ( -0.000000000000000000, -1.000000000000000000, -0.000000000000000000 ) ) ;
#14427 = DIRECTION ( 'NONE',  ( 0.000000000000000000, 0.000000000000000000, 1.000000000000000000 ) ) ;
#14428 = LINE ( 'NONE', #8046, #14682 ) ;
#14429 = ADVANCED_FACE ( 'NONE', ( #6667 ), #1453, .T. ) ;
#14430 = FACE_OUTER_BOUND ( 'NONE', #15908, .T. ) ;
#14431 =( NAMED_UNIT ( * ) PLANE_ANGLE_UNIT ( ) SI_UNIT ( $, .RADIAN. ) );
#14432 = FILL_AREA_STYLE_COLOUR ( '', #15063 ) ;
#14433 = EDGE_CURVE ( 'NONE', #3463, #10515, #3354, .T. ) ;
#14434 = CARTESIAN_POINT ( 'NONE',  ( -79.99999999999995737, 146.8256012863087676, 507.0490161104376057 ) ) ;
#14435 = EDGE_CURVE ( 'NONE', #8449, #13105, #3799, .T. ) ;
#14436 = LINE ( 'NONE', #18856, #13646 ) ;
#14437 = FACE_OUTER_BOUND ( 'NONE', #8131, .T. ) ;
#14438 = VECTOR ( 'NONE', #12825, 1000.000000000000000 ) ;
#14439 = VERTEX_POINT ( 'NONE', #5125 ) ;
#14440 = ORIENTED_EDGE ( 'NONE', *, *, #3625, .F. ) ;
#14441 = CARTESIAN_POINT ( 'NONE',  ( 111.4893729001365870, 222.0013992467745823, 330.1364716053970483 ) ) ;
#14442 = EDGE_LOOP ( 'NONE', ( #8823, #3783, #13566, #16747, #3293, #10312, #13778, #17673 ) ) ;
#14443 = DIRECTION ( 'NONE',  ( -0.000000000000000000, -1.000000000000000000, -0.000000000000000000 ) ) ;
#14444 = CARTESIAN_POINT ( 'NONE',  ( 22.99999999999999645, 68.00000000000000000, 31.00000000000006750 ) ) ;
#14445 = VERTEX_POINT ( 'NONE', #1795 ) ;
#14446 = CARTESIAN_POINT ( 'NONE',  ( -39.99999999999999289, 11.00000000000000000, -34.99999999999997868 ) ) ;
#14447 = VECTOR ( 'NONE', #19985, 1000.000000000000000 ) ;
#14448 = CARTESIAN_POINT ( 'NONE',  ( 30.99999999999999645, 0.000000000000000000, 31.00000000000001066 ) ) ;
#14449 = DIRECTION ( 'NONE',  ( 1.000000000000000000, 0.000000000000000000, 0.000000000000000000 ) ) ;
#14450 = CIRCLE ( 'NONE', #6568, 10.00000000000000888 ) ;
#14451 = EDGE_CURVE ( 'NONE', #4371, #6655, #5773, .T. ) ;
#14452 = CARTESIAN_POINT ( 'NONE',  ( -0.5803134113676365891, 139.9120960380916188, 501.0815185958381335 ) ) ;
#14453 = CARTESIAN_POINT ( 'NONE',  ( 78.48937290013660117, 123.1299228374914208, 29.36128450348865471 ) ) ;
#14454 = CARTESIAN_POINT ( 'NONE',  ( -79.99999999999995737, 316.7545334744432921, 205.1946179577815883 ) ) ;
#14455 = CARTESIAN_POINT ( 'NONE',  ( -80.12104746910925712, 139.8955315650537443, 489.0596075541194523 ) ) ;
#14456 = ORIENTED_EDGE ( 'NONE', *, *, #9735, .T. ) ;
#14457 = DIRECTION ( 'NONE',  ( -6.123031769111888756E-17, 1.000000000000000000, 3.749151804555346336E-33 ) ) ;
#14458 = CARTESIAN_POINT ( 'NONE',  ( -44.50085094405410757, 209.4098724938429541, 510.3921618609452935 ) ) ;
#14459 = CARTESIAN_POINT ( 'NONE',  ( -23.00000000000000000, 0.000000000000000000, -31.00000000000005684 ) ) ;
#14460 = ADVANCED_FACE ( 'NONE', ( #12847 ), #14074, .F. ) ;
#14461 = CARTESIAN_POINT ( 'NONE',  ( -81.18192946989245229, 147.7545334744432921, 491.0690926367356042 ) ) ;
#14462 = APPLICATION_CONTEXT ( 'automotive_design' ) ;
#14463 = ORIENTED_EDGE ( 'NONE', *, *, #12946, .T. ) ;
#14464 = VECTOR ( 'NONE', #10176, 1000.000000000000000 ) ;
#14465 = EDGE_LOOP ( 'NONE', ( #17205, #18205, #8781, #7564 ) ) ;
#14466 = AXIS2_PLACEMENT_3D ( 'NONE', #9996, #1846, #16308 ) ;
#14467 = STYLED_ITEM ( 'NONE', ( #15227 ), #5498 ) ;
#14468 = VERTEX_POINT ( 'NONE', #1574 ) ;
#14469 = ORIENTED_EDGE ( 'NONE', *, *, #13431, .F. ) ;
#14470 = FACE_BOUND ( 'NONE', #730, .T. ) ;
#14471 = PRESENTATION_STYLE_ASSIGNMENT (( #9739 ) ) ;
#14472 = ORIENTED_EDGE ( 'NONE', *, *, #10178, .F. ) ;
#14473 = DIRECTION ( 'NONE',  ( 0.000000000000000000, 1.000000000000000000, 0.000000000000000000 ) ) ;
#14474 = DIRECTION ( 'NONE',  ( 0.000000000000000000, 1.000000000000000000, 0.000000000000000000 ) ) ;
#14475 = ORIENTED_EDGE ( 'NONE', *, *, #8600, .T. ) ;
#14476 =( LENGTH_UNIT ( ) NAMED_UNIT ( * ) SI_UNIT ( .MILLI., .METRE. ) );
#14477 = CARTESIAN_POINT ( 'NONE',  ( 178.4893729001365728, 113.1299228374914918, 220.6387154965113382 ) ) ;
#14478 = AXIS2_PLACEMENT_3D ( 'NONE', #19007, #20151, #4608 ) ;
#14479 = VECTOR ( 'NONE', #6479, 1000.000000000000000 ) ;
#14480 = ADVANCED_FACE ( 'NONE', ( #17270 ), #4692, .F. ) ;
#14481 = VECTOR ( 'NONE', #3955, 1000.000000000000000 ) ;
#14482 = CARTESIAN_POINT ( 'NONE',  ( 78.48937290013660117, 113.1299228374914208, 29.36128450348865471 ) ) ;
#14483 = ORIENTED_EDGE ( 'NONE', *, *, #10250, .F. ) ;
#14484 = LINE ( 'NONE', #7997, #19118 ) ;
#14485 = FACE_OUTER_BOUND ( 'NONE', #9985, .T. ) ;
#14486 = ORIENTED_EDGE ( 'NONE', *, *, #16313, .T. ) ;
#14487 = FILL_AREA_STYLE_COLOUR ( '', #18461 ) ;
#14488 = ORIENTED_EDGE ( 'NONE', *, *, #4070, .T. ) ;
#14489 = VERTEX_POINT ( 'NONE', #13073 ) ;
#14490 = VECTOR ( 'NONE', #5958, 1000.000000000000000 ) ;
#14491 = CIRCLE ( 'NONE', #16483, 10.00000000000000178 ) ;
#14492 = AXIS2_PLACEMENT_3D ( 'NONE', #11461, #19181, #5287 ) ;
#14493 = EDGE_LOOP ( 'NONE', ( #199, #2612, #4281, #15279 ) ) ;
#14494 = CARTESIAN_POINT ( 'NONE',  ( -80.70993973863717486, 139.4861549367042528, 500.2186618843511496 ) ) ;
#14495 = ADVANCED_FACE ( 'NONE', ( #13368 ), #10241, .F. ) ;
#14496 = ORIENTED_EDGE ( 'NONE', *, *, #954, .F. ) ;
#14497 = LINE ( 'NONE', #16277, #4442 ) ;
#14498 = AXIS2_PLACEMENT_3D ( 'NONE', #2245, #14839, #11449 ) ;
#14499 = ORIENTED_EDGE ( 'NONE', *, *, #11001, .F. ) ;
#14500 = LINE ( 'NONE', #12980, #1271 ) ;
#14501 = CARTESIAN_POINT ( 'NONE',  ( 0.000000000000000000, 216.7545334744432921, 515.1946179577817020 ) ) ;
#14502 = FACE_OUTER_BOUND ( 'NONE', #8905, .T. ) ;
#14503 = CARTESIAN_POINT ( 'NONE',  ( 0.000000000000000000, 138.7545334744432637, 510.3921618609452935 ) ) ;
#14504 = PRESENTATION_LAYER_ASSIGNMENT (  '', '', ( #3659 ) ) ;
#14505 = CARTESIAN_POINT ( 'NONE',  ( 498.8117674897343932, 191.8198460455371333, 235.0057801310552463 ) ) ;
#14506 =( NAMED_UNIT ( * ) SI_UNIT ( $, .STERADIAN. ) SOLID_ANGLE_UNIT ( ) );
#14507 = AXIS2_PLACEMENT_3D ( 'NONE', #9523, #251, #6552 ) ;
#14508 = CARTESIAN_POINT ( 'NONE',  ( 31.00000000000002842, 68.00000000000000000, 23.00000000000001066 ) ) ;
#14509 = ADVANCED_FACE ( 'NONE', ( #19501 ), #3869, .F. ) ;
#14510 = CARTESIAN_POINT ( 'NONE',  ( -34.99999999999996447, 11.00000000000000000, 40.00000000000000711 ) ) ;
#14511 = CARTESIAN_POINT ( 'NONE',  ( 498.8117674897343932, 214.2156642432025251, 250.0000000000000000 ) ) ;
#14512 = LINE ( 'NONE', #2020, #14464 ) ;
#14513 = VERTEX_POINT ( 'NONE', #2293 ) ;
#14514 = PRODUCT_RELATED_PRODUCT_CATEGORY ( 'part', '', ( #7599 ) ) ;
#14515 = VERTEX_POINT ( 'NONE', #15002 ) ;
#14516 = ORIENTED_EDGE ( 'NONE', *, *, #9237, .T. ) ;
#14517 = VERTEX_POINT ( 'NONE', #8589 ) ;
#14518 = ORIENTED_EDGE ( 'NONE', *, *, #7653, .T. ) ;
#14519 = EDGE_CURVE ( 'NONE', #16393, #6961, #11804, .T. ) ;
#14520 = AXIS2_PLACEMENT_3D ( 'NONE', #9160, #6672, #1895 ) ;
#14521 = FACE_OUTER_BOUND ( 'NONE', #5700, .T. ) ;
#14522 = PRESENTATION_LAYER_ASSIGNMENT (  '', '', ( #2997 ) ) ;
#14523 =( NAMED_UNIT ( * ) SI_UNIT ( $, .STERADIAN. ) SOLID_ANGLE_UNIT ( ) );
#14524 = FACE_OUTER_BOUND ( 'NONE', #10719, .T. ) ;
#14525 = PLANE ( 'NONE',  #17309 ) ;
#14526 = DIRECTION ( 'NONE',  ( 0.000000000000000000, 1.000000000000000000, 0.000000000000000000 ) ) ;
#14527 = CARTESIAN_POINT ( 'NONE',  ( 2.999999999999996891, 60.00000000000000711, 9.013878188659974811 ) ) ;
#14528 = CARTESIAN_POINT ( 'NONE',  ( 1.574999999999999956, 0.000000000000000000, 0.000000000000000000 ) ) ;
#14529 = CARTESIAN_POINT ( 'NONE',  ( 39.99999999999999289, 10.00000000000000000, 26.00000000000000000 ) ) ;
#14530 = EDGE_CURVE ( 'NONE', #13299, #6793, #13248, .T. ) ;
#14531 = CARTESIAN_POINT ( 'NONE',  ( 0.000000000000000000, 0.000000000000000000, -135.0000000000000284 ) ) ;
#14532 = EDGE_CURVE ( 'NONE', #6793, #16010, #5607, .T. ) ;
#14533 = CARTESIAN_POINT ( 'NONE',  ( 4.899999999999999467, -12.00000000000000000, 1.509263698769704680E-15 ) ) ;
#14534 = CARTESIAN_POINT ( 'NONE',  ( -79.99999999999995737, 139.7733885855926701, 501.8237260975782874 ) ) ;
#14535 =( GEOMETRIC_REPRESENTATION_CONTEXT ( 3 ) GLOBAL_UNCERTAINTY_ASSIGNED_CONTEXT ( ( #11973 ) ) GLOBAL_UNIT_ASSIGNED_CONTEXT ( ( #12051, #7700, #14389 ) ) REPRESENTATION_CONTEXT ( 'NONE', 'WORKASPACE' ) );
#14536 = EDGE_CURVE ( 'NONE', #715, #6120, #3127, .T. ) ;
#14537 = MECHANICAL_DESIGN_GEOMETRIC_PRESENTATION_REPRESENTATION (  '', ( #19783 ), #6978 ) ;
#14538 = EDGE_CURVE ( 'NONE', #506, #18058, #4781, .T. ) ;
#14539 = ORIENTED_EDGE ( 'NONE', *, *, #2961, .F. ) ;
#14540 = CARTESIAN_POINT ( 'NONE',  ( 53.48937290013659407, 167.9162550801369491, 0.000000000000000000 ) ) ;
#14541 = ORIENTED_EDGE ( 'NONE', *, *, #10043, .T. ) ;
#14542 = ADVANCED_FACE ( 'NONE', ( #2404 ), #1987, .T. ) ;
#14543 = ORIENTED_EDGE ( 'NONE', *, *, #7351, .T. ) ;
#14544 = ADVANCED_FACE ( 'NONE', ( #11489 ), #16968, .T. ) ;
#14545 = DIRECTION ( 'NONE',  ( -1.000000000000000000, 0.000000000000000000, -0.000000000000000000 ) ) ;
#14546 = PRESENTATION_LAYER_ASSIGNMENT (  '', '', ( #7974 ) ) ;
#14547 = PLANE ( 'NONE',  #1923 ) ;
#14548 = ORIENTED_EDGE ( 'NONE', *, *, #15391, .F. ) ;
#14549 = LINE ( 'NONE', #17647, #3149 ) ;
#14550 = CARTESIAN_POINT ( 'NONE',  ( -31.00000000000005684, 68.00000000000000000, 23.00000000000000355 ) ) ;
#14551 = DIRECTION ( 'NONE',  ( 0.000000000000000000, 0.000000000000000000, -1.000000000000000000 ) ) ;
#14552 = LINE ( 'NONE', #2378, #6857 ) ;
#14553 = CYLINDRICAL_SURFACE ( 'NONE', #15495, 1.000000000000000888 ) ;
#14554 =( GEOMETRIC_REPRESENTATION_CONTEXT ( 3 ) GLOBAL_UNCERTAINTY_ASSIGNED_CONTEXT ( ( #19541 ) ) GLOBAL_UNIT_ASSIGNED_CONTEXT ( ( #5342, #13101, #17902 ) ) REPRESENTATION_CONTEXT ( 'NONE', 'WORKASPACE' ) );
#14555 = EDGE_CURVE ( 'NONE', #18007, #53, #14779, .T. ) ;
#14556 = ORIENTED_EDGE ( 'NONE', *, *, #13174, .T. ) ;
#14557 = FACE_OUTER_BOUND ( 'NONE', #20050, .T. ) ;
#14558 = DIRECTION ( 'NONE',  ( 0.000000000000000000, 0.000000000000000000, 1.000000000000000000 ) ) ;
#14559 = CARTESIAN_POINT ( 'NONE',  ( 1.181929469893326257, 140.4048636633015406, 500.8237260975781737 ) ) ;
#14560 = CARTESIAN_POINT ( 'NONE',  ( -1.776356839400249676E-15, 15.90000000000000036, 0.000000000000000000 ) ) ;
#14561 = CIRCLE ( 'NONE', #17194, 10.00000000000000888 ) ;
#14562 = EDGE_LOOP ( 'NONE', ( #18864, #829, #10015, #10908 ) ) ;
#14563 = COLOUR_RGB ( '', 0.31764706, 0.68627451, 0.89019608) ;
#14564 = ORIENTED_EDGE ( 'NONE', *, *, #7811, .T. ) ;
#14565 = EDGE_CURVE ( 'NONE', #9586, #19903, #16259, .T. ) ;
#14566 = ORIENTED_EDGE ( 'NONE', *, *, #9394, .F. ) ;
#14567 = CYLINDRICAL_SURFACE ( 'NONE', #19593, 2.999999999999995559 ) ;
#14568 = CYLINDRICAL_SURFACE ( 'NONE', #7048, 10.00000000000000888 ) ;
#14569 = AXIS2_PLACEMENT_3D ( 'NONE', #18702, #3034, #3251 ) ;
#14570 = ORIENTED_EDGE ( 'NONE', *, *, #4038, .T. ) ;
#14571 = AXIS2_PLACEMENT_3D ( 'NONE', #12801, #14122, #1429 ) ;
#14572 = CARTESIAN_POINT ( 'NONE',  ( 35.00000000000000711, 8.000000000000000000, -35.00000000000000711 ) ) ;
#14573 = EDGE_CURVE ( 'NONE', #5865, #2482, #2097, .T. ) ;
#14574 = CYLINDRICAL_SURFACE ( 'NONE', #15802, 15.25000000000000000 ) ;
#14575 = VERTEX_POINT ( 'NONE', #15302 ) ;
#14576 = DIRECTION ( 'NONE',  ( 0.000000000000000000, 0.000000000000000000, -1.000000000000000000 ) ) ;
#14577 = AXIS2_PLACEMENT_3D ( 'NONE', #13040, #19295, #13134 ) ;
#14578 = LINE ( 'NONE', #11982, #10611 ) ;
#14579 = DIRECTION ( 'NONE',  ( 1.000000000000000000, 0.000000000000000000, -0.000000000000000000 ) ) ;
#14580 = LINE ( 'NONE', #3870, #932 ) ;
#14581 = DIRECTION ( 'NONE',  ( 1.000000000000000000, 0.000000000000000000, 0.000000000000000000 ) ) ;
#14582 = ORIENTED_EDGE ( 'NONE', *, *, #2246, .F. ) ;
#14583 = DIRECTION ( 'NONE',  ( 0.000000000000000000, 0.000000000000000000, 1.000000000000000000 ) ) ;
#14584 = LINE ( 'NONE', #15461, #14844 ) ;
#14585 = DIRECTION ( 'NONE',  ( -0.000000000000000000, 0.7817866094812263578, 0.6235460666509320404 ) ) ;
#14586 = DIRECTION ( 'NONE',  ( -1.000000000000000000, -0.000000000000000000, -0.000000000000000000 ) ) ;
#14587 =( NAMED_UNIT ( * ) PLANE_ANGLE_UNIT ( ) SI_UNIT ( $, .RADIAN. ) );
#14588 = CLOSED_SHELL ( 'NONE', ( #16376, #4004, #9578, #17573, #7238, #19301, #18459, #10883, #18322, #2545, #13061, #16080, #16712, #4924, #2949, #12371, #15608, #3313, #16744, #930, #1709, #12909, #10139, #12671, #15379, #15054 ) ) ;
#14589 = DIRECTION ( 'NONE',  ( 0.000000000000000000, 0.000000000000000000, 1.000000000000000000 ) ) ;
#14590 = VECTOR ( 'NONE', #6694, 1000.000000000000000 ) ;
#14591 = SURFACE_SIDE_STYLE ('',( #12966 ) ) ;
#14592 = ORIENTED_EDGE ( 'NONE', *, *, #13580, .F. ) ;
#14593 = EDGE_LOOP ( 'NONE', ( #9208, #19087 ) ) ;
#14594 = AXIS2_PLACEMENT_3D ( 'NONE', #2911, #1338, #15517 ) ;
#14595 = AXIS2_PLACEMENT_3D ( 'NONE', #7018, #13304, #14735 ) ;
#14596 = EDGE_CURVE ( 'NONE', #19875, #3145, #19910, .T. ) ;
#14597 = ORIENTED_EDGE ( 'NONE', *, *, #11764, .F. ) ;
#14598 = DIRECTION ( 'NONE',  ( 0.000000000000000000, 1.000000000000000000, 0.000000000000000000 ) ) ;
#14599 = DIRECTION ( 'NONE',  ( 0.000000000000000000, -1.000000000000000000, 0.000000000000000000 ) ) ;
#14600 = VERTEX_POINT ( 'NONE', #7473 ) ;
#14601 = DIRECTION ( 'NONE',  ( 0.000000000000000000, 0.000000000000000000, 1.000000000000000000 ) ) ;
#14602 = STYLED_ITEM ( 'NONE', ( #5314 ), #1264 ) ;
#14603 = AXIS2_PLACEMENT_3D ( 'NONE', #1419, #12081, #7445 ) ;
#14604 =( GEOMETRIC_REPRESENTATION_CONTEXT ( 3 ) GLOBAL_UNCERTAINTY_ASSIGNED_CONTEXT ( ( #5764 ) ) GLOBAL_UNIT_ASSIGNED_CONTEXT ( ( #17375, #15960, #263 ) ) REPRESENTATION_CONTEXT ( 'NONE', 'WORKASPACE' ) );
#14605 = ORIENTED_EDGE ( 'NONE', *, *, #13547, .T. ) ;
#14606 = PLANE ( 'NONE',  #11860 ) ;
#14607 = DIRECTION ( 'NONE',  ( 1.000000000000000000, 9.815121534730717399E-17, 0.000000000000000000 ) ) ;
#14608 = DIRECTION ( 'NONE',  ( -6.120180426682198458E-17, 0.6235460666509320404, -0.7817866094812263578 ) ) ;
#14609 = CARTESIAN_POINT ( 'NONE',  ( 423.8334540492694487, 191.8198460455371333, 34.99421986894476788 ) ) ;
#14610 = DIRECTION ( 'NONE',  ( 0.000000000000000000, 0.000000000000000000, -1.000000000000000000 ) ) ;
#14611 = AXIS2_PLACEMENT_3D ( 'NONE', #19755, #12068, #13707 ) ;
#14612 = AXIS2_PLACEMENT_3D ( 'NONE', #11684, #19393, #5297 ) ;
#14614 = MECHANICAL_DESIGN_GEOMETRIC_PRESENTATION_REPRESENTATION (  '', ( #17950 ), #8041 ) ;
#14613 = DIRECTION ( 'NONE',  ( 0.000000000000000000, 2.352167425053297897E-16, 1.000000000000000000 ) ) ;
#14615 = AXIS2_PLACEMENT_3D ( 'NONE', #4312, #7606, #10592 ) ;
#14616 = CARTESIAN_POINT ( 'NONE',  ( 25.99999999999999645, 68.00000000000000000, 31.00000000000004619 ) ) ;
#14617 = MECHANICAL_DESIGN_GEOMETRIC_PRESENTATION_REPRESENTATION (  '', ( #3095 ), #9344 ) ;
#14618 = DIRECTION ( 'NONE',  ( -0.000000000000000000, 1.000000000000000000, -0.000000000000000000 ) ) ;
#14619 = VERTEX_POINT ( 'NONE', #15508 ) ;
#14620 = SURFACE_SIDE_STYLE ('',( #16394 ) ) ;
#14621 = FILL_AREA_STYLE_COLOUR ( '', #15464 ) ;
#14622 = VERTEX_POINT ( 'NONE', #10351 ) ;
#14623 = TOROIDAL_SURFACE ( 'NONE', #6411, 8.000000000000000000, 1.000000000000000000 ) ;
#14624 = AXIS2_PLACEMENT_3D ( 'NONE', #10590, #13782, #7212 ) ;
#14625 = VERTEX_POINT ( 'NONE', #8808 ) ;
#14626 = STYLED_ITEM ( 'NONE', ( #12523 ), #10139 ) ;
#14627 = ORIENTED_EDGE ( 'NONE', *, *, #11532, .F. ) ;
#14628 = EDGE_CURVE ( 'NONE', #18411, #15133, #6788, .T. ) ;
#14629 = ORIENTED_EDGE ( 'NONE', *, *, #18645, .F. ) ;
#14630 = ORIENTED_EDGE ( 'NONE', *, *, #4078, .T. ) ;
#14631 = AXIS2_PLACEMENT_3D ( 'NONE', #14482, #5318, #7993 ) ;
#14632 = CARTESIAN_POINT ( 'NONE',  ( 25.99999999999997868, 8.000000000000000000, -39.99999999999999289 ) ) ;
#14633 = LINE ( 'NONE', #17718, #774 ) ;
#14634 =( GEOMETRIC_REPRESENTATION_CONTEXT ( 3 ) GLOBAL_UNCERTAINTY_ASSIGNED_CONTEXT ( ( #9910 ) ) GLOBAL_UNIT_ASSIGNED_CONTEXT ( ( #7028, #8364, #521 ) ) REPRESENTATION_CONTEXT ( 'NONE', 'WORKASPACE' ) );
#14635 = PLANE ( 'NONE',  #14595 ) ;
#14636 = CARTESIAN_POINT ( 'NONE',  ( -1.274252908074454287E-14, 138.8810201506713611, 488.5655098179835818 ) ) ;
#14637 =( GEOMETRIC_REPRESENTATION_CONTEXT ( 3 ) GLOBAL_UNCERTAINTY_ASSIGNED_CONTEXT ( ( #10345 ) ) GLOBAL_UNIT_ASSIGNED_CONTEXT ( ( #2788, #20087, #1201 ) ) REPRESENTATION_CONTEXT ( 'NONE', 'WORKASPACE' ) );
#14638 = CARTESIAN_POINT ( 'NONE',  ( 31.00000000000003553, 19.00000000000000000, 20.99999999999999289 ) ) ;
#14639 = CARTESIAN_POINT ( 'NONE',  ( 1.983673311716144694, 62.25902922769662240, 9.291669371308648451 ) ) ;
#14640 = STYLED_ITEM ( 'NONE', ( #11824 ), #827 ) ;
#14641 = DIRECTION ( 'NONE',  ( -1.000000000000000000, 0.000000000000000000, 0.000000000000000000 ) ) ;
#14642 = DIRECTION ( 'NONE',  ( -5.827381659956976845E-17, 0.5937146717273790175, 0.8046756418431283420 ) ) ;
#14643 = DIRECTION ( 'NONE',  ( -0.000000000000000000, -1.000000000000000000, -0.000000000000000000 ) ) ;
#14644 = CYLINDRICAL_SURFACE ( 'NONE', #4383, 36.00000000000000000 ) ;
#14645 = EDGE_CURVE ( 'NONE', #8331, #12278, #2610, .T. ) ;
#14646 = CARTESIAN_POINT ( 'NONE',  ( 0.000000000000000000, 66.00000000000000000, 0.000000000000000000 ) ) ;
#14647 = MECHANICAL_DESIGN_GEOMETRIC_PRESENTATION_REPRESENTATION (  '', ( #1450 ), #13021 ) ;
#14648 = ORIENTED_EDGE ( 'NONE', *, *, #17332, .F. ) ;
#14649 = STYLED_ITEM ( 'NONE', ( #16513 ), #1960 ) ;
#14650 = CIRCLE ( 'NONE', #4134, 17.85000000000000142 ) ;
#14651 = UNCERTAINTY_MEASURE_WITH_UNIT (LENGTH_MEASURE( 1.000000000000000082E-05 ), #15966, 'distance_accuracy_value', 'NONE');
#14652 = ORIENTED_EDGE ( 'NONE', *, *, #13257, .F. ) ;
#14653 = PRESENTATION_LAYER_ASSIGNMENT (  '', '', ( #12035 ) ) ;
#14654 = EDGE_CURVE ( 'NONE', #738, #14402, #19802, .T. ) ;
#14655 = PLANE ( 'NONE',  #19436 ) ;
#14656 = VERTEX_POINT ( 'NONE', #13743 ) ;
#14657 = UNCERTAINTY_MEASURE_WITH_UNIT (LENGTH_MEASURE( 1.000000000000000082E-05 ), #14861, 'distance_accuracy_value', 'NONE');
#14658 = DIRECTION ( 'NONE',  ( -0.000000000000000000, 0.000000000000000000, 1.000000000000000000 ) ) ;
#14659 = FACE_OUTER_BOUND ( 'NONE', #13327, .T. ) ;
#14660 = UNCERTAINTY_MEASURE_WITH_UNIT (LENGTH_MEASURE( 1.000000000000000082E-05 ), #19557, 'distance_accuracy_value', 'NONE');
#14661 = ORIENTED_EDGE ( 'NONE', *, *, #431, .T. ) ;
#14662 = LINE ( 'NONE', #9715, #509 ) ;
#14663 = DIRECTION ( 'NONE',  ( 0.000000000000000000, 0.000000000000000000, -1.000000000000000000 ) ) ;
#14664 = VECTOR ( 'NONE', #6019, 1000.000000000000000 ) ;
#14665 = CARTESIAN_POINT ( 'NONE',  ( 35.99999999999999289, 10.00000000000000000, 18.99999999999999289 ) ) ;
#14666 = EDGE_CURVE ( 'NONE', #5319, #5083, #9538, .T. ) ;
#14667 = CARTESIAN_POINT ( 'NONE',  ( 30.99999999999997513, 0.000000000000000000, 30.99999999999999645 ) ) ;
#14668 = FILL_AREA_STYLE ('',( #14862 ) ) ;
#14669 = COLOUR_RGB ( '', 0.66274510, 0.83137255, 0.94901961) ;
#14670 = LINE ( 'NONE', #8566, #12193 ) ;
#14671 = LINE ( 'NONE', #11372, #7416 ) ;
#14672 = ORIENTED_EDGE ( 'NONE', *, *, #10982, .F. ) ;
#14673 = FACE_BOUND ( 'NONE', #19972, .T. ) ;
#14674 = DIRECTION ( 'NONE',  ( 1.000000000000000000, 0.000000000000000000, 0.000000000000000000 ) ) ;
#14675 = CARTESIAN_POINT ( 'NONE',  ( 2.181929469892980755, 139.7545334744432637, 496.6642397995873921 ) ) ;
#14676 = VECTOR ( 'NONE', #9322, 1000.000000000000000 ) ;
#14677 = EDGE_CURVE ( 'NONE', #13902, #15829, #5913, .T. ) ;
#14678 = ADVANCED_FACE ( 'NONE', ( #4068 ), #941, .T. ) ;
#14679 = ORIENTED_EDGE ( 'NONE', *, *, #1577, .F. ) ;
#14680 = ORIENTED_EDGE ( 'NONE', *, *, #757, .T. ) ;
#14681 = ORIENTED_EDGE ( 'NONE', *, *, #4335, .T. ) ;
#14682 = VECTOR ( 'NONE', #14335, 1000.000000000000000 ) ;
#14683 = CARTESIAN_POINT ( 'NONE',  ( 2.799999999999999822, -13.30000000000000071, -1.628780242865979955E-15 ) ) ;
#14684 = EDGE_CURVE ( 'NONE', #15351, #7754, #2904, .T. ) ;
#14685 = ORIENTED_EDGE ( 'NONE', *, *, #13133, .T. ) ;
#14686 = UNCERTAINTY_MEASURE_WITH_UNIT (LENGTH_MEASURE( 1.000000000000000082E-05 ), #10498, 'distance_accuracy_value', 'NONE');
#14687 = DIRECTION ( 'NONE',  ( 6.123031769111888756E-17, 0.000000000000000000, 1.000000000000000000 ) ) ;
#14688 = CARTESIAN_POINT ( 'NONE',  ( 2.693790225569809849, 39.66504951222130870, 9.110418847747206783 ) ) ;
#14689 = ORIENTED_EDGE ( 'NONE', *, *, #5776, .F. ) ;
#14690 = CARTESIAN_POINT ( 'NONE',  ( -26.00000000000002132, 8.000000000000000000, 40.00000000000000711 ) ) ;
#14691 = CARTESIAN_POINT ( 'NONE',  ( -26.00000000000002132, 0.000000000000000000, -39.99999999999999289 ) ) ;
#14692 = LINE ( 'NONE', #8877, #19492 ) ;
#14693 = CARTESIAN_POINT ( 'NONE',  ( 0.000000000000000000, 8.000000000000000000, 0.000000000000000000 ) ) ;
#14694 = EDGE_CURVE ( 'NONE', #10459, #8530, #1035, .T. ) ;
#14695 = DIRECTION ( 'NONE',  ( 1.000000000000000000, -0.000000000000000000, 0.000000000000000000 ) ) ;
#14696 = ORIENTED_EDGE ( 'NONE', *, *, #11288, .F. ) ;
#14697 = LINE ( 'NONE', #13252, #4557 ) ;
#14698 =( NAMED_UNIT ( * ) SI_UNIT ( $, .STERADIAN. ) SOLID_ANGLE_UNIT ( ) );
#14699 = LINE ( 'NONE', #359, #6684 ) ;
#14700 = DIRECTION ( 'NONE',  ( -1.000000000000000000, 0.000000000000000000, 0.000000000000000000 ) ) ;
#14701 = CARTESIAN_POINT ( 'NONE',  ( -365.3332378693668829, 113.0853859501458345, 214.9384415106391089 ) ) ;
#14702 = ADVANCED_FACE ( 'NONE', ( #2813 ), #1331, .T. ) ;
#14703 = CIRCLE ( 'NONE', #2505, 10.00000000000000178 ) ;
#14704 = EDGE_LOOP ( 'NONE', ( #6980, #6073, #12517, #20074 ) ) ;
#14705 = DIRECTION ( 'NONE',  ( 0.000000000000000000, 0.000000000000000000, -1.000000000000000000 ) ) ;
#14706 = VERTEX_POINT ( 'NONE', #10752 ) ;
#14707 = ORIENTED_EDGE ( 'NONE', *, *, #1162, .T. ) ;
#14708 = ORIENTED_EDGE ( 'NONE', *, *, #17227, .F. ) ;
#14709 = DIRECTION ( 'NONE',  ( -0.000000000000000000, -1.000000000000000000, -0.000000000000000000 ) ) ;
#14710 = ORIENTED_EDGE ( 'NONE', *, *, #7388, .F. ) ;
#14711 = DIRECTION ( 'NONE',  ( -0.000000000000000000, 0.000000000000000000, 1.000000000000000000 ) ) ;
#14712 = DIRECTION ( 'NONE',  ( 0.000000000000000000, 0.000000000000000000, 1.000000000000000000 ) ) ;
#14713 = EDGE_CURVE ( 'NONE', #1029, #11272, #7663, .T. ) ;
#14714 = ORIENTED_EDGE ( 'NONE', *, *, #3969, .F. ) ;
#14715 = SURFACE_SIDE_STYLE ('',( #776 ) ) ;
#14716 = CARTESIAN_POINT ( 'NONE',  ( 25.99999999999999645, 68.00000000000000000, 40.00000000000002132 ) ) ;
#14717 = CARTESIAN_POINT ( 'NONE',  ( 0.8610374118361808771, 138.8314847497733524, 489.5655098155585279 ) ) ;
#14718 =( LENGTH_UNIT ( ) NAMED_UNIT ( * ) SI_UNIT ( .MILLI., .METRE. ) );
#14719 = CARTESIAN_POINT ( 'NONE',  ( -1.242741617435013895E-14, 216.7545334744432921, 501.8237260975781737 ) ) ;
#14720 = EDGE_CURVE ( 'NONE', #18268, #13692, #2144, .T. ) ;
#14721 = DIRECTION ( 'NONE',  ( 0.000000000000000000, 0.000000000000000000, -1.000000000000000000 ) ) ;
#14722 = LINE ( 'NONE', #284, #16871 ) ;
#14723 = CARTESIAN_POINT ( 'NONE',  ( 423.8334540492694487, 191.8198460455371333, 91.76606011801541740 ) ) ;
#14724 =( NAMED_UNIT ( * ) SI_UNIT ( $, .STERADIAN. ) SOLID_ANGLE_UNIT ( ) );
#14725 = ORIENTED_EDGE ( 'NONE', *, *, #17062, .F. ) ;
#14726 =( GEOMETRIC_REPRESENTATION_CONTEXT ( 3 ) GLOBAL_UNCERTAINTY_ASSIGNED_CONTEXT ( ( #5211 ) ) GLOBAL_UNIT_ASSIGNED_CONTEXT ( ( #3522, #3304, #15893 ) ) REPRESENTATION_CONTEXT ( 'NONE', 'WORKASPACE' ) );
#14727 = ORIENTED_EDGE ( 'NONE', *, *, #13938, .F. ) ;
#14728 = ORIENTED_EDGE ( 'NONE', *, *, #11411, .T. ) ;
#14729 = ORIENTED_EDGE ( 'NONE', *, *, #914, .T. ) ;
#14730 = ORIENTED_EDGE ( 'NONE', *, *, #950, .T. ) ;
#14731 = DIRECTION ( 'NONE',  ( 0.000000000000000000, 0.000000000000000000, -1.000000000000000000 ) ) ;
#14732 = DIRECTION ( 'NONE',  ( -0.000000000000000000, 1.000000000000000000, -0.000000000000000000 ) ) ;
#14733 = CARTESIAN_POINT ( 'NONE',  ( 53.48937290013659407, 129.7247684487574588, 370.0000000000000000 ) ) ;
#14734 = EDGE_CURVE ( 'NONE', #4219, #12468, #16663, .T. ) ;
#14735 = DIRECTION ( 'NONE',  ( 3.854941057726251409E-16, 0.000000000000000000, 1.000000000000000000 ) ) ;
#14736 = AXIS2_PLACEMENT_3D ( 'NONE', #4985, #3011, #12820 ) ;
#14737 = LINE ( 'NONE', #17627, #10505 ) ;
#14738 = CARTESIAN_POINT ( 'NONE',  ( 2.799999999999999822, 0.000000000000000000, 0.000000000000000000 ) ) ;
#14739 = CARTESIAN_POINT ( 'NONE',  ( 1.507804506096818820, 62.60084458484482894, 9.381017998102993971 ) ) ;
#14740 = CARTESIAN_POINT ( 'NONE',  ( 31.00000000000000000, 19.00000000000000000, -21.00000000000000355 ) ) ;
#14741 = APPLICATION_CONTEXT ( 'automotive_design' ) ;
#14742 = CARTESIAN_POINT ( 'NONE',  ( 149.0892156028631348, 80.91625508013694912, 245.0000000000000000 ) ) ;
#14743 = EDGE_CURVE ( 'NONE', #18280, #17493, #16756, .T. ) ;
#14744 = LINE ( 'NONE', #14534, #4430 ) ;
#14745 = VERTEX_POINT ( 'NONE', #13546 ) ;
#14746 = VECTOR ( 'NONE', #16982, 1000.000000000000000 ) ;
#14747 = CARTESIAN_POINT ( 'NONE',  ( 498.8117674897343932, 191.8198460455371333, 215.0057801310552179 ) ) ;
#14748 = VERTEX_POINT ( 'NONE', #9720 ) ;
#14749 = ORIENTED_EDGE ( 'NONE', *, *, #17667, .F. ) ;
#14750 = DIRECTION ( 'NONE',  ( 0.000000000000000000, 0.000000000000000000, 1.000000000000000000 ) ) ;
#14751 = CARTESIAN_POINT ( 'NONE',  ( -20.99999999999999645, 19.00000000000000000, 35.00000000000001421 ) ) ;
#14752 = CYLINDRICAL_SURFACE ( 'NONE', #6238, 10.00000000000000888 ) ;
#14753 = ORIENTED_EDGE ( 'NONE', *, *, #17356, .T. ) ;
#14754 = EDGE_CURVE ( 'NONE', #13719, #6685, #122, .T. ) ;
#14755 = LINE ( 'NONE', #14857, #186 ) ;
#14756 = DIRECTION ( 'NONE',  ( -0.000000000000000000, 1.000000000000000000, -0.000000000000000000 ) ) ;
#14757 = DIRECTION ( 'NONE',  ( 1.000000000000000000, 0.000000000000000000, 0.000000000000000000 ) ) ;
#14758 = PLANE ( 'NONE',  #15158 ) ;
#14759 = DIRECTION ( 'NONE',  ( -1.000000000000000000, -0.000000000000000000, -0.000000000000000000 ) ) ;
#14760 = CIRCLE ( 'NONE', #7530, 5.000000000000004441 ) ;
#14761 = ORIENTED_EDGE ( 'NONE', *, *, #7789, .F. ) ;
#14762 = PRESENTATION_STYLE_ASSIGNMENT (( #17658 ) ) ;
#14763 = CARTESIAN_POINT ( 'NONE',  ( 40.00000000000000711, 19.00000000000000000, -26.00000000000000355 ) ) ;
#14764 = CYLINDRICAL_SURFACE ( 'NONE', #19215, 18.50000000000000000 ) ;
#14765 = ADVANCED_FACE ( 'NONE', ( #6325 ), #16067, .T. ) ;
#14766 = PRODUCT_DEFINITION ( 'UNKNOWN', '', #6013, #18102 ) ;
#14767 = VERTEX_POINT ( 'NONE', #8182 ) ;
#14768 = ORIENTED_EDGE ( 'NONE', *, *, #10339, .F. ) ;
#14769 = DIRECTION ( 'NONE',  ( 1.000000000000000000, 0.000000000000000000, -0.000000000000000000 ) ) ;
#14770 =( GEOMETRIC_REPRESENTATION_CONTEXT ( 3 ) GLOBAL_UNCERTAINTY_ASSIGNED_CONTEXT ( ( #3759 ) ) GLOBAL_UNIT_ASSIGNED_CONTEXT ( ( #7160, #4350, #10534 ) ) REPRESENTATION_CONTEXT ( 'NONE', 'WORKASPACE' ) );
#14772 = ORIENTED_EDGE ( 'NONE', *, *, #6986, .T. ) ;
#14771 = AXIS2_PLACEMENT_3D ( 'NONE', #18064, #9947, #3964 ) ;
#14773 = CARTESIAN_POINT ( 'NONE',  ( 0.8615489040082175975, 139.7703989349544713, 489.5655098179837523 ) ) ;
#14774 = ORIENTED_EDGE ( 'NONE', *, *, #16210, .T. ) ;
#14775 = CARTESIAN_POINT ( 'NONE',  ( 53.48937290013660828, 127.7247684487574304, 254.0000000000000000 ) ) ;
#14776 = CARTESIAN_POINT ( 'NONE',  ( -40.00000000000000711, 8.000000000000000000, -19.00000000000000355 ) ) ;
#14777 = SURFACE_SIDE_STYLE ('',( #17563 ) ) ;
#14778 = EDGE_CURVE ( 'NONE', #18686, #4266, #4144, .T. ) ;
#14779 = LINE ( 'NONE', #17771, #1123 ) ;
#14780 = DIRECTION ( 'NONE',  ( 0.000000000000000000, -0.7071067811865753283, 0.7071067811865198172 ) ) ;
#14781 = DIRECTION ( 'NONE',  ( 1.000000000000000000, 0.000000000000000000, -0.000000000000000000 ) ) ;
#14782 = ORIENTED_EDGE ( 'NONE', *, *, #62, .T. ) ;
#14783 = DIRECTION ( 'NONE',  ( 0.000000000000000000, -1.000000000000000000, 0.000000000000000000 ) ) ;
#14784 = DIRECTION ( 'NONE',  ( 0.000000000000000000, 0.000000000000000000, -1.000000000000000000 ) ) ;
#14785 = SURFACE_STYLE_USAGE ( .BOTH. , #17779 ) ;
#14786 =( NAMED_UNIT ( * ) PLANE_ANGLE_UNIT ( ) SI_UNIT ( $, .RADIAN. ) );
#14787 = CIRCLE ( 'NONE', #5906, 7.999999999999996447 ) ;
#14788 = ADVANCED_FACE ( 'NONE', ( #20321, #17132, #4667 ), #10958, .F. ) ;
#14789 = SURFACE_STYLE_USAGE ( .BOTH. , #17985 ) ;
#14790 = AXIS2_PLACEMENT_3D ( 'NONE', #16874, #9227, #10882 ) ;
#14791 = EDGE_LOOP ( 'NONE', ( #7972, #13751, #10425, #9743 ) ) ;
#14792 = EDGE_CURVE ( 'NONE', #1444, #13434, #11048, .T. ) ;
#14793 = VERTEX_POINT ( 'NONE', #6753 ) ;
#14794 = EDGE_CURVE ( 'NONE', #4680, #10259, #3848, .T. ) ;
#14795 = EDGE_LOOP ( 'NONE', ( #13001, #15130, #17744, #17403 ) ) ;
#14796 = ORIENTED_EDGE ( 'NONE', *, *, #15707, .F. ) ;
#14797 = DIRECTION ( 'NONE',  ( -0.000000000000000000, -1.000000000000000000, -0.000000000000000000 ) ) ;
#14798 = LINE ( 'NONE', #871, #3847 ) ;
#14799 = EDGE_LOOP ( 'NONE', ( #8507, #5480, #11993, #10285 ) ) ;
#14800 = EDGE_CURVE ( 'NONE', #16197, #7139, #17750, .T. ) ;
#14801 = VECTOR ( 'NONE', #16282, 1000.000000000000000 ) ;
#14802 = DIRECTION ( 'NONE',  ( 1.000000000000000000, -0.000000000000000000, -0.000000000000000000 ) ) ;
#14803 = CIRCLE ( 'NONE', #7242, 8.000000000000000000 ) ;
#14804 = CARTESIAN_POINT ( 'NONE',  ( -1.776356839400249676E-15, 13.94999999999999929, 0.000000000000000000 ) ) ;
#14805 = ORIENTED_EDGE ( 'NONE', *, *, #14684, .T. ) ;
#14806 = DIRECTION ( 'NONE',  ( -1.000000000000000000, -9.815121534730717399E-17, 0.000000000000000000 ) ) ;
#14807 = FACE_OUTER_BOUND ( 'NONE', #19442, .T. ) ;
#14808 = CARTESIAN_POINT ( 'NONE',  ( -1.000000000000012657, 140.8764026050585869, 502.4686618848270996 ) ) ;
#14809 = LINE ( 'NONE', #14609, #18538 ) ;
#14810 = DIRECTION ( 'NONE',  ( 0.000000000000000000, -1.000000000000000000, 0.000000000000000000 ) ) ;
#14811 = FACE_OUTER_BOUND ( 'NONE', #5647, .T. ) ;
#14812 = CARTESIAN_POINT ( 'NONE',  ( -31.81980515339462912, 8.000000000000000000, 28.51980515339464972 ) ) ;
#14813 =( NAMED_UNIT ( * ) PLANE_ANGLE_UNIT ( ) SI_UNIT ( $, .RADIAN. ) );
#14814 = VERTEX_POINT ( 'NONE', #19385 ) ;
#14815 = AXIS2_PLACEMENT_3D ( 'NONE', #19451, #5358, #4006 ) ;
#14816 = VERTEX_POINT ( 'NONE', #5494 ) ;
#14817 = PRODUCT_DEFINITION_CONTEXT ( 'detailed design', #17633, 'design' ) ;
#14818 = PRODUCT_DEFINITION_CONTEXT ( 'detailed design', #10922, 'design' ) ;
#14819 = ORIENTED_EDGE ( 'NONE', *, *, #19544, .F. ) ;
#14820 = ORIENTED_EDGE ( 'NONE', *, *, #17336, .T. ) ;
#14821 = EDGE_LOOP ( 'NONE', ( #8751, #2511, #10723, #8110 ) ) ;
#14822 = EDGE_CURVE ( 'NONE', #12943, #11592, #19477, .T. ) ;
#14823 = CARTESIAN_POINT ( 'NONE',  ( -79.05444436839837863, 139.0463324665402070, 488.7916445138383210 ) ) ;
#14824 = CYLINDRICAL_SURFACE ( 'NONE', #12997, 10.00000000000000888 ) ;
#14825 = CARTESIAN_POINT ( 'NONE',  ( 53.48937290013659407, 145.9162550801369491, 250.0000000000000000 ) ) ;
#14826 = EDGE_CURVE ( 'NONE', #12399, #6575, #5090, .T. ) ;
#14827 = DIRECTION ( 'NONE',  ( 0.000000000000000000, 0.000000000000000000, 1.000000000000000000 ) ) ;
#14828 = LINE ( 'NONE', #10493, #17760 ) ;
#14829 =( GEOMETRIC_REPRESENTATION_CONTEXT ( 3 ) GLOBAL_UNCERTAINTY_ASSIGNED_CONTEXT ( ( #2253 ) ) GLOBAL_UNIT_ASSIGNED_CONTEXT ( ( #1235, #6025, #14146 ) ) REPRESENTATION_CONTEXT ( 'NONE', 'WORKASPACE' ) );
#14830 = EDGE_CURVE ( 'NONE', #5907, #1869, #19902, .T. ) ;
#14831 = LINE ( 'NONE', #14636, #6819 ) ;
#14832 = CIRCLE ( 'NONE', #1983, 2.500000000000002220 ) ;
#14833 = SURFACE_STYLE_FILL_AREA ( #8650 ) ;
#14834 = AXIS2_PLACEMENT_3D ( 'NONE', #842, #8879, #5805 ) ;
#14835 = FACE_OUTER_BOUND ( 'NONE', #18788, .T. ) ;
#14836 = DIRECTION ( 'NONE',  ( 0.000000000000000000, 0.000000000000000000, -1.000000000000000000 ) ) ;
#14837 = DIRECTION ( 'NONE',  ( 0.000000000000000000, 0.000000000000000000, 1.000000000000000000 ) ) ;
#14838 = CARTESIAN_POINT ( 'NONE',  ( -78.99999999999995737, 139.2066006846527841, 488.2525619656395861 ) ) ;
#14839 = DIRECTION ( 'NONE',  ( 1.000000000000000000, -0.000000000000000000, 0.000000000000000000 ) ) ;
#14840 =( GEOMETRIC_REPRESENTATION_CONTEXT ( 3 ) GLOBAL_UNCERTAINTY_ASSIGNED_CONTEXT ( ( #3736 ) ) GLOBAL_UNIT_ASSIGNED_CONTEXT ( ( #8161, #9802, #1943 ) ) REPRESENTATION_CONTEXT ( 'NONE', 'WORKASPACE' ) );
#14841 = DIRECTION ( 'NONE',  ( 1.000000000000000000, 0.000000000000000000, 0.000000000000000000 ) ) ;
#14842 = LINE ( 'NONE', #707, #2112 ) ;
#14843 = ORIENTED_EDGE ( 'NONE', *, *, #13900, .T. ) ;
#14844 = VECTOR ( 'NONE', #18643, 1000.000000000000000 ) ;
#14845 = VECTOR ( 'NONE', #499, 1000.000000000000000 ) ;
#14846 = CIRCLE ( 'NONE', #20102, 10.00000000000000888 ) ;
#14847 = ORIENTED_EDGE ( 'NONE', *, *, #10178, .T. ) ;
#14848 = LINE ( 'NONE', #13325, #7087 ) ;
#14849 = UNCERTAINTY_MEASURE_WITH_UNIT (LENGTH_MEASURE( 1.000000000000000082E-05 ), #1512, 'distance_accuracy_value', 'NONE');
#14850 = VERTEX_POINT ( 'NONE', #13042 ) ;
#14851 = ORIENTED_EDGE ( 'NONE', *, *, #642, .T. ) ;
#14852 = ORIENTED_EDGE ( 'NONE', *, *, #3429, .F. ) ;
#14853 = ADVANCED_FACE ( 'NONE', ( #19189 ), #13341, .F. ) ;
#14854 = DIRECTION ( 'NONE',  ( -1.000000000000000000, 0.000000000000000000, 0.000000000000000000 ) ) ;
#14855 = UNCERTAINTY_MEASURE_WITH_UNIT (LENGTH_MEASURE( 1.000000000000000082E-05 ), #14718, 'distance_accuracy_value', 'NONE');
#14856 = EDGE_LOOP ( 'NONE', ( #10767, #1222 ) ) ;
#14857 = CARTESIAN_POINT ( 'NONE',  ( 423.8334540492694487, 191.8198460455371333, 71.76606011801538898 ) ) ;
#14858 = CARTESIAN_POINT ( 'NONE',  ( -23.00000000000002487, 10.00000000000000000, -31.00000000000003553 ) ) ;
#14859 = LINE ( 'NONE', #7047, #7022 ) ;
#14860 = VECTOR ( 'NONE', #760, 1000.000000000000000 ) ;
#14861 =( LENGTH_UNIT ( ) NAMED_UNIT ( * ) SI_UNIT ( .MILLI., .METRE. ) );
#14862 = FILL_AREA_STYLE_COLOUR ( '', #13444 ) ;
#14863 = DIRECTION ( 'NONE',  ( -0.000000000000000000, -1.000000000000000000, -0.000000000000000000 ) ) ;
#14864 = CARTESIAN_POINT ( 'NONE',  ( 10.00000000000000000, 5.352861011586007481E-13, -75.00000000000599698 ) ) ;
#14865 =( GEOMETRIC_REPRESENTATION_CONTEXT ( 3 ) GLOBAL_UNCERTAINTY_ASSIGNED_CONTEXT ( ( #5051 ) ) GLOBAL_UNIT_ASSIGNED_CONTEXT ( ( #7262, #13543, #2399 ) ) REPRESENTATION_CONTEXT ( 'NONE', 'WORKASPACE' ) );
#14866 = ORIENTED_EDGE ( 'NONE', *, *, #15471, .F. ) ;
#14867 = FACE_OUTER_BOUND ( 'NONE', #2850, .T. ) ;
#14868 = SURFACE_STYLE_FILL_AREA ( #18047 ) ;
#14869 = FACE_OUTER_BOUND ( 'NONE', #10987, .T. ) ;
#14870 = ORIENTED_EDGE ( 'NONE', *, *, #2630, .F. ) ;
#14871 = ORIENTED_EDGE ( 'NONE', *, *, #11764, .T. ) ;
#14872 = VECTOR ( 'NONE', #5102, 1000.000000000000000 ) ;
#14873 = AXIS2_PLACEMENT_3D ( 'NONE', #5442, #484, #11728 ) ;
#14874 = ORIENTED_EDGE ( 'NONE', *, *, #18821, .T. ) ;
#14875 = LINE ( 'NONE', #6866, #3432 ) ;
#14876 = CARTESIAN_POINT ( 'NONE',  ( -211.5106270998635409, 123.1299228374912644, 79.58252780074349175 ) ) ;
#14877 = UNCERTAINTY_MEASURE_WITH_UNIT (LENGTH_MEASURE( 1.000000000000000082E-05 ), #14476, 'distance_accuracy_value', 'NONE');
#14878 = EDGE_LOOP ( 'NONE', ( #20338, #10203, #2896, #9382, #17714, #3410 ) ) ;
#14879 =( NAMED_UNIT ( * ) PLANE_ANGLE_UNIT ( ) SI_UNIT ( $, .RADIAN. ) );
#14880 = CARTESIAN_POINT ( 'NONE',  ( 1.181929469892980755, 147.7545334744432921, 496.6642397995874489 ) ) ;
#14881 = VECTOR ( 'NONE', #8922, 1000.000000000000000 ) ;
#14882 = CARTESIAN_POINT ( 'NONE',  ( -211.5106270998635409, 103.1299228374912360, 29.36128450348865471 ) ) ;
#14883 = DIRECTION ( 'NONE',  ( 0.000000000000000000, 0.000000000000000000, -1.000000000000000000 ) ) ;
#14884 = CARTESIAN_POINT ( 'NONE',  ( 10.00000000000000000, 309.2289037985885898, -79.88019484660914316 ) ) ;
#14885 = ORIENTED_EDGE ( 'NONE', *, *, #8810, .F. ) ;
#14886 = DIRECTION ( 'NONE',  ( -0.000000000000000000, 0.7817866094812263578, 0.6235460666509320404 ) ) ;
#14887 = CARTESIAN_POINT ( 'NONE',  ( 0.000000000000000000, 216.7545334744432921, 512.1946179577817020 ) ) ;
#14888 = DIRECTION ( 'NONE',  ( -0.000000000000000000, -1.000000000000000000, -0.000000000000000000 ) ) ;
#14889 = SURFACE_STYLE_USAGE ( .BOTH. , #18068 ) ;
#14890 = CIRCLE ( 'NONE', #5351, 9.500000000000000000 ) ;
#14891 = AXIS2_PLACEMENT_3D ( 'NONE', #7998, #17162, #163 ) ;
#14892 = CYLINDRICAL_SURFACE ( 'NONE', #9995, 10.00000000000000888 ) ;
#14893 = CARTESIAN_POINT ( 'NONE',  ( 230.9893729001384486, -274.0243638824161962, 101.5415023676493291 ) ) ;
#14894 = EDGE_LOOP ( 'NONE', ( #6257, #14319, #5910, #15513 ) ) ;
#14895 = CARTESIAN_POINT ( 'NONE',  ( 463.8334540492693350, 191.8198460455371333, 91.76606011801541740 ) ) ;
#14896 = CIRCLE ( 'NONE', #13588, 0.6999999999999992895 ) ;
#14897 = EDGE_CURVE ( 'NONE', #11272, #4354, #10529, .T. ) ;
#14898 = VERTEX_POINT ( 'NONE', #2585 ) ;
#14899 = ORIENTED_EDGE ( 'NONE', *, *, #11236, .F. ) ;
#14900 = PRODUCT_DEFINITION_FORMATION_WITH_SPECIFIED_SOURCE ( 'ANY', '', #17662, .NOT_KNOWN. ) ;
#14901 = VECTOR ( 'NONE', #9437, 1000.000000000000000 ) ;
#14902 = ORIENTED_EDGE ( 'NONE', *, *, #19290, .T. ) ;
#14903 = EDGE_LOOP ( 'NONE', ( #8757, #14214, #13731, #1561, #18174, #7597 ) ) ;
#14904 = VERTEX_POINT ( 'NONE', #8792 ) ;
#14905 = PRESENTATION_STYLE_ASSIGNMENT (( #9294 ) ) ;
#14906 = VECTOR ( 'NONE', #5892, 1000.000000000000000 ) ;
#14907 = CARTESIAN_POINT ( 'NONE',  ( 21.00000000000000000, 8.000000000000000000, -31.00000000000003908 ) ) ;
#14908 = AXIS2_PLACEMENT_3D ( 'NONE', #16584, #2439, #8743 ) ;
#14909 = ORIENTED_EDGE ( 'NONE', *, *, #16601, .T. ) ;
#14910 = LINE ( 'NONE', #17995, #18585 ) ;
#14911 = EDGE_CURVE ( 'NONE', #7206, #15689, #4345, .T. ) ;
#14912 = SURFACE_STYLE_USAGE ( .BOTH. , #8615 ) ;
#14913 = VECTOR ( 'NONE', #5512, 1000.000000000000000 ) ;
#14914 = DIRECTION ( 'NONE',  ( 6.123031769111888756E-17, -1.000000000000000000, -3.749151804555344967E-33 ) ) ;
#14915 = CARTESIAN_POINT ( 'NONE',  ( -31.00000000000002842, 0.000000000000000000, -25.99999999999999645 ) ) ;
#14916 = FACE_OUTER_BOUND ( 'NONE', #13468, .T. ) ;
#14917 = DIRECTION ( 'NONE',  ( 1.000000000000000000, 9.815121534730717399E-17, 0.000000000000000000 ) ) ;
#14918 = CLOSED_SHELL ( 'NONE', ( #14460, #9410, #3334, #19831, #20267, #17419, #13472, #10226, #18365, #13068, #16831, #5242, #3130, #2683, #19092, #7903, #5787, #2566, #18727, #4736, #7850, #2261, #2549, #15286, #2670, #16593, #16435, #8562, #16703, #6208, #3190, #1154, #6383, #15006, #8391, #11103, #4323, #10359, #10512, #18063, #10971, #2198, #10018, #13922, #12786, #15735, #9660, #16990, #18939, #6895, #11812, #19177, #11538, #15056, #15357, #4961 ) ) ;
#14919 = ADVANCED_FACE ( 'NONE', ( #13621 ), #12086, .F. ) ;
#14920 = DIRECTION ( 'NONE',  ( -1.000000000000000000, -2.135044278125301096E-16, -0.000000000000000000 ) ) ;
#14921 =( NAMED_UNIT ( * ) SI_UNIT ( $, .STERADIAN. ) SOLID_ANGLE_UNIT ( ) );
#14922 = PRESENTATION_STYLE_ASSIGNMENT (( #16693 ) ) ;
#14923 = EDGE_CURVE ( 'NONE', #7205, #16010, #7340, .T. ) ;
#14924 = CARTESIAN_POINT ( 'NONE',  ( -1.000000000000012657, 139.2066006846527841, 488.2525619656395861 ) ) ;
#14925 =( NAMED_UNIT ( * ) PLANE_ANGLE_UNIT ( ) SI_UNIT ( $, .RADIAN. ) );
#14926 = UNCERTAINTY_MEASURE_WITH_UNIT (LENGTH_MEASURE( 1.000000000000000082E-05 ), #17213, 'distance_accuracy_value', 'NONE');
#14927 = CYLINDRICAL_SURFACE ( 'NONE', #9249, 10.00000000000000888 ) ;
#14928 = CARTESIAN_POINT ( 'NONE',  ( 498.8334540492693918, 214.2156642432025251, 250.0000000000000000 ) ) ;
#14929 = VECTOR ( 'NONE', #20298, 1000.000000000000227 ) ;
#14930 = ORIENTED_EDGE ( 'NONE', *, *, #13919, .T. ) ;
#14931 = VECTOR ( 'NONE', #15959, 1000.000000000000000 ) ;
#14932 = ADVANCED_FACE ( 'NONE', ( #5994 ), #11880, .T. ) ;
#14933 = ORIENTED_EDGE ( 'NONE', *, *, #5362, .F. ) ;
#14934 = ORIENTED_EDGE ( 'NONE', *, *, #11079, .F. ) ;
#14935 = PRESENTATION_LAYER_ASSIGNMENT (  '', '', ( #11652 ) ) ;
#14936 = ORIENTED_EDGE ( 'NONE', *, *, #13441, .T. ) ;
#14937 = CARTESIAN_POINT ( 'NONE',  ( -79.01070358830934026, 139.1212506049081981, 488.5223375167593076 ) ) ;
#14938 = FACE_OUTER_BOUND ( 'NONE', #18384, .T. ) ;
#14939 = DIRECTION ( 'NONE',  ( 0.000000000000000000, 0.000000000000000000, 1.000000000000000000 ) ) ;
#14940 = EDGE_CURVE ( 'NONE', #10796, #2901, #13728, .T. ) ;
#14941 =( LENGTH_UNIT ( ) NAMED_UNIT ( * ) SI_UNIT ( .MILLI., .METRE. ) );
#14942 = VECTOR ( 'NONE', #11206, 1000.000000000000000 ) ;
#14943 = VECTOR ( 'NONE', #7803, 1000.000000000000000 ) ;
#14944 = FILL_AREA_STYLE ('',( #18324 ) ) ;
#14945 = CARTESIAN_POINT ( 'NONE',  ( 31.00000000000006395, 68.00000000000000000, -22.99999999999999289 ) ) ;
#14946 = PRESENTATION_STYLE_ASSIGNMENT (( #19559 ) ) ;
#14947 = CARTESIAN_POINT ( 'NONE',  ( 458.8334540492693350, 191.8198460455371333, 24.99421986894476078 ) ) ;
#14948 = SURFACE_SIDE_STYLE ('',( #15141 ) ) ;
#14949 = DIRECTION ( 'NONE',  ( -5.889072920838430686E-16, 1.000000000000000000, -0.000000000000000000 ) ) ;
#14950 = DIRECTION ( 'NONE',  ( 0.000000000000000000, 1.000000000000000000, 0.000000000000000000 ) ) ;
#14951 = ADVANCED_FACE ( 'NONE', ( #1012 ), #19890, .F. ) ;
#14952 = FACE_BOUND ( 'NONE', #13992, .T. ) ;
#14953 = CIRCLE ( 'NONE', #3100, 2.000000000000001776 ) ;
#14954 = CIRCLE ( 'NONE', #15287, 4.999999999999997335 ) ;
#14955 = CARTESIAN_POINT ( 'NONE',  ( 31.81980515339464333, 0.000000000000000000, -28.51980515339463906 ) ) ;
#14956 = LINE ( 'NONE', #2565, #1104 ) ;
#14957 = EDGE_CURVE ( 'NONE', #12424, #10365, #13968, .T. ) ;
#14958 = EDGE_LOOP ( 'NONE', ( #146, #15390, #13177, #2416, #14729, #8602, #2649, #14486 ) ) ;
#14959 = COLOUR_RGB ( '', 0.72549020, 0.75294118, 0.79215686) ;
#14960 = ORIENTED_EDGE ( 'NONE', *, *, #10288, .T. ) ;
#14961 = AXIS2_PLACEMENT_3D ( 'NONE', #10992, #9445, #1581 ) ;
#14962 = DIRECTION ( 'NONE',  ( 1.000000000000000000, 0.000000000000000000, -0.000000000000000000 ) ) ;
#14963 = VERTEX_POINT ( 'NONE', #7454 ) ;
#14964 = ORIENTED_EDGE ( 'NONE', *, *, #16300, .F. ) ;
#14965 = PRESENTATION_LAYER_ASSIGNMENT (  '', '', ( #8397 ) ) ;
#14966 = PLANE ( 'NONE',  #17231 ) ;
#14967 = FACE_OUTER_BOUND ( 'NONE', #15405, .T. ) ;
#14968 = COLOUR_RGB ( '', 0.08235294, 0.09019608, 0.10196078) ;
#14969 = VERTEX_POINT ( 'NONE', #7543 ) ;
#14970 = PRESENTATION_LAYER_ASSIGNMENT (  '', '', ( #18246 ) ) ;
#14971 = CARTESIAN_POINT ( 'NONE',  ( 498.8334540492693918, 191.8198460455371333, 235.0057801310552463 ) ) ;
#14972 = CARTESIAN_POINT ( 'NONE',  ( 53.48937290013660828, 127.7247684487574304, 357.7985149490353933 ) ) ;
#14973 = CARTESIAN_POINT ( 'NONE',  ( 10.00000000000000000, 372.8685141053778693, -79.88019484660868841 ) ) ;
#14974 = ADVANCED_FACE ( 'NONE', ( #19989 ), #5895, .F. ) ;
#14975 = AXIS2_PLACEMENT_3D ( 'NONE', #127, #11067, #13138 ) ;
#14976 = VECTOR ( 'NONE', #6529, 1000.000000000000000 ) ;
#14977 = CARTESIAN_POINT ( 'NONE',  ( 463.8334540492693350, 214.2156642432025251, 0.000000000000000000 ) ) ;
#14978 = FACE_OUTER_BOUND ( 'NONE', #8683, .T. ) ;
#14979 = FACE_OUTER_BOUND ( 'NONE', #13251, .T. ) ;
#14980 = AXIS2_PLACEMENT_3D ( 'NONE', #8772, #16806, #15254 ) ;
#14981 = PLANE ( 'NONE',  #1801 ) ;
#14982 = EDGE_CURVE ( 'NONE', #14090, #16534, #2888, .T. ) ;
#14983 = ORIENTED_EDGE ( 'NONE', *, *, #18691, .F. ) ;
#14984 = SURFACE_STYLE_USAGE ( .BOTH. , #3944 ) ;
#14985 = AXIS2_PLACEMENT_3D ( 'NONE', #19766, #8664, #7325 ) ;
#14986 = VECTOR ( 'NONE', #18608, 1000.000000000000000 ) ;
#14987 = PRESENTATION_LAYER_ASSIGNMENT (  '', '', ( #8066 ) ) ;
#14988 = EDGE_LOOP ( 'NONE', ( #8039, #4889, #289, #5924 ) ) ;
#14989 = VECTOR ( 'NONE', #9463, 1000.000000000000000 ) ;
#14990 = ORIENTED_EDGE ( 'NONE', *, *, #10891, .F. ) ;
#14991 = CIRCLE ( 'NONE', #6108, 8.000000000000000000 ) ;
#14992 = AXIS2_PLACEMENT_3D ( 'NONE', #14693, #11589, #18062 ) ;
#14993 = ORIENTED_EDGE ( 'NONE', *, *, #5329, .F. ) ;
#14994 = FILL_AREA_STYLE_COLOUR ( '', #4427 ) ;
#14995 = CARTESIAN_POINT ( 'NONE',  ( 35.00000000000000711, 11.00000000000000000, 35.00000000000000711 ) ) ;
#14996 = VERTEX_POINT ( 'NONE', #9092 ) ;
#14997 = DIRECTION ( 'NONE',  ( -0.000000000000000000, 1.000000000000000000, -0.000000000000000000 ) ) ;
#14998 = CARTESIAN_POINT ( 'NONE',  ( -78.99999999999995737, 147.7545334744432921, 491.0690926367356042 ) ) ;
#14999 =( NAMED_UNIT ( * ) SI_UNIT ( $, .STERADIAN. ) SOLID_ANGLE_UNIT ( ) );
#15000 = UNCERTAINTY_MEASURE_WITH_UNIT (LENGTH_MEASURE( 1.000000000000000082E-05 ), #16980, 'distance_accuracy_value', 'NONE');
#15001 = VECTOR ( 'NONE', #12113, 1000.000000000000000 ) ;
#15002 = CARTESIAN_POINT ( 'NONE',  ( 25.99999999999998224, 10.00000000000000000, -32.99999999999999289 ) ) ;
#15003 = PLANE ( 'NONE',  #5429 ) ;
#15004 = ORIENTED_EDGE ( 'NONE', *, *, #9379, .T. ) ;
#15005 = CARTESIAN_POINT ( 'NONE',  ( 1.347066989204613998E-15, 0.000000000000000000, 22.00000000000000000 ) ) ;
#15006 = ADVANCED_FACE ( 'NONE', ( #15382 ), #840, .T. ) ;
#15007 = ORIENTED_EDGE ( 'NONE', *, *, #13851, .F. ) ;
#15008 = ORIENTED_EDGE ( 'NONE', *, *, #9406, .F. ) ;
#15009 = ORIENTED_EDGE ( 'NONE', *, *, #847, .T. ) ;
#15010 = MANIFOLD_SOLID_BREP ( 'Cut-Extrude1', #17219 ) ;
#15011 = VECTOR ( 'NONE', #304, 1000.000000000000000 ) ;
#15012 = B_SPLINE_CURVE_WITH_KNOTS ( 'NONE', 3,
 ( #3107, #20095, #9, #13823, #12586, #10737, #15706, #2890, #5996, #15488, #6310, #10943, #12275, #9179 ),
 .UNSPECIFIED., .F., .F.,
 ( 4, 2, 2, 2, 2, 2, 4 ),
 ( 0.000000000000000000, 0.0009284677239257688175, 0.001856935447851537635, 0.002321169309814422044, 0.002785403171777306452, 0.003249637033740190861, 0.003713870895703075270 ),
 .UNSPECIFIED. ) ;
#15013 = VERTEX_POINT ( 'NONE', #6308 ) ;
#15014 = ORIENTED_EDGE ( 'NONE', *, *, #17099, .F. ) ;
#15015 = DIRECTION ( 'NONE',  ( 0.000000000000000000, 0.000000000000000000, -1.000000000000000000 ) ) ;
#15016 = LINE ( 'NONE', #13475, #5182 ) ;
#15017 = ORIENTED_EDGE ( 'NONE', *, *, #14792, .T. ) ;
#15018 = EDGE_CURVE ( 'NONE', #1451, #5387, #15703, .T. ) ;
#15019 = CARTESIAN_POINT ( 'NONE',  ( 111.4893729001366154, 77.72476844875745883, 250.0000000000000000 ) ) ;
#15020 = PLANE ( 'NONE',  #12246 ) ;
#15021 = VECTOR ( 'NONE', #18111, 1000.000000000000000 ) ;
#15022 = CARTESIAN_POINT ( 'NONE',  ( 0.1271853858195616527, 139.8992328697892162, 489.0579231335084955 ) ) ;
#15023 =( NAMED_UNIT ( * ) PLANE_ANGLE_UNIT ( ) SI_UNIT ( $, .RADIAN. ) );
#15024 = FACE_OUTER_BOUND ( 'NONE', #14465, .T. ) ;
#15025 = CARTESIAN_POINT ( 'NONE',  ( -39.99999999999999289, 11.00000000000000000, 25.99999999999999645 ) ) ;
#15026 = MECHANICAL_DESIGN_GEOMETRIC_PRESENTATION_REPRESENTATION (  '', ( #5478 ), #16034 ) ;
#15027 =( NAMED_UNIT ( * ) SI_UNIT ( $, .STERADIAN. ) SOLID_ANGLE_UNIT ( ) );
#15028 =( LENGTH_UNIT ( ) NAMED_UNIT ( * ) SI_UNIT ( .MILLI., .METRE. ) );
#15029 = FILL_AREA_STYLE_COLOUR ( '', #8324 ) ;
#15030 = DIRECTION ( 'NONE',  ( -0.000000000000000000, 0.000000000000000000, 1.000000000000000000 ) ) ;
#15031 = SURFACE_SIDE_STYLE ('',( #8748 ) ) ;
#15032 = CYLINDRICAL_SURFACE ( 'NONE', #6268, 18.49999999999998934 ) ;
#15033 = ORIENTED_EDGE ( 'NONE', *, *, #19685, .T. ) ;
#15034 = EDGE_CURVE ( 'NONE', #15689, #16657, #10941, .T. ) ;
#15035 = ORIENTED_EDGE ( 'NONE', *, *, #7247, .T. ) ;
#15036 = PRODUCT_DEFINITION_CONTEXT ( 'detailed design', #13432, 'design' ) ;
#15037 = EDGE_LOOP ( 'NONE', ( #8298, #17400 ) ) ;
#15038 = EDGE_CURVE ( 'NONE', #16331, #9586, #1310, .T. ) ;
#15039 = ORIENTED_EDGE ( 'NONE', *, *, #13851, .T. ) ;
#15040 = VECTOR ( 'NONE', #16570, 1000.000000000000000 ) ;
#15041 = DIRECTION ( 'NONE',  ( 1.000000000000000000, 5.889072920838430686E-16, -0.000000000000000000 ) ) ;
#15042 = FACE_OUTER_BOUND ( 'NONE', #10585, .T. ) ;
#15043 = DIRECTION ( 'NONE',  ( 1.000000000000000000, -0.000000000000000000, -0.000000000000000000 ) ) ;
#15044 = CARTESIAN_POINT ( 'NONE',  ( 0.000000000000000000, 316.7545334744432353, 495.1946179577816451 ) ) ;
#15045 = FILL_AREA_STYLE_COLOUR ( '', #9426 ) ;
#15046 = CARTESIAN_POINT ( 'NONE',  ( -82.18192946989277914, 138.7545334744432637, 500.8237260975782874 ) ) ;
#15047 = LINE ( 'NONE', #11956, #10118 ) ;
#15048 = EDGE_CURVE ( 'NONE', #10793, #5054, #10831, .T. ) ;
#15049 = CARTESIAN_POINT ( 'NONE',  ( -25.99999999999999645, 68.00000000000000000, 40.00000000000002132 ) ) ;
#15050 = SURFACE_STYLE_FILL_AREA ( #4138 ) ;
#15051 = PLANE ( 'NONE',  #8576 ) ;
#15052 = CARTESIAN_POINT ( 'NONE',  ( 26.00000000000000000, 19.00000000000000000, 40.00000000000001421 ) ) ;
#15053 = CARTESIAN_POINT ( 'NONE',  ( -23.00000000000002487, 0.000000000000000000, -31.00000000000003553 ) ) ;
#15054 = ADVANCED_FACE ( 'NONE', ( #15791 ), #7749, .F. ) ;
#15055 = ORIENTED_EDGE ( 'NONE', *, *, #5226, .F. ) ;
#15056 = ADVANCED_FACE ( 'NONE', ( #13923, #14120 ), #17508, .T. ) ;
#15057 = DIRECTION ( 'NONE',  ( -0.7327934916262990317, -0.6804510993672779895, -8.333122608164345406E-17 ) ) ;
#15058 = ORIENTED_EDGE ( 'NONE', *, *, #11177, .F. ) ;
#15059 = ORIENTED_EDGE ( 'NONE', *, *, #6809, .T. ) ;
#15060 = EDGE_CURVE ( 'NONE', #4349, #16025, #6109, .T. ) ;
#15061 = ORIENTED_EDGE ( 'NONE', *, *, #17944, .T. ) ;
#15062 = CARTESIAN_POINT ( 'NONE',  ( -19.00000000000001776, 8.000000000000000000, 40.00000000000000711 ) ) ;
#15063 = COLOUR_RGB ( '', 0.08235294, 0.09019608, 0.10196078) ;
#15064 = DIRECTION ( 'NONE',  ( -1.000000000000000000, 0.000000000000000000, 0.000000000000000000 ) ) ;
#15065 = FILL_AREA_STYLE_COLOUR ( '', #20363 ) ;
#15066 = ADVANCED_FACE ( 'NONE', ( #17634 ), #3523, .F. ) ;
#15067 = LINE ( 'NONE', #8561, #3817 ) ;
#15068 = DIRECTION ( 'NONE',  ( 1.000000000000000000, 0.000000000000000000, 0.000000000000000000 ) ) ;
#15069 = DIRECTION ( 'NONE',  ( 0.000000000000000000, 0.000000000000000000, 1.000000000000000000 ) ) ;
#15070 = ADVANCED_FACE ( 'NONE', ( #404 ), #2037, .T. ) ;
#15071 =( NAMED_UNIT ( * ) SI_UNIT ( $, .STERADIAN. ) SOLID_ANGLE_UNIT ( ) );
#15072 = SURFACE_SIDE_STYLE ('',( #18551 ) ) ;
#15073 = DIRECTION ( 'NONE',  ( 0.000000000000000000, 1.000000000000000000, 0.000000000000000000 ) ) ;
#15074 = CARTESIAN_POINT ( 'NONE',  ( -81.00000000000258638, 138.7723821175183900, 490.5025619656395861 ) ) ;
#15075 = DIRECTION ( 'NONE',  ( 0.000000000000000000, 1.000000000000000000, 7.137148015447440312E-15 ) ) ;
#15076 = VERTEX_POINT ( 'NONE', #518 ) ;
#15077 =( NAMED_UNIT ( * ) PLANE_ANGLE_UNIT ( ) SI_UNIT ( $, .RADIAN. ) );
#15078 = VECTOR ( 'NONE', #1551, 1000.000000000000000 ) ;
#15079 = DIRECTION ( 'NONE',  ( -0.9740972002433518906, 0.2261297071993489949, 0.000000000000000000 ) ) ;
#15080 = CIRCLE ( 'NONE', #9464, 3.883636366625808911 ) ;
#15081 = ORIENTED_EDGE ( 'NONE', *, *, #17713, .T. ) ;
#15082 = ORIENTED_EDGE ( 'NONE', *, *, #2318, .F. ) ;
#15083 = ADVANCED_FACE ( 'NONE', ( #16211 ), #6616, .T. ) ;
#15084 = DIRECTION ( 'NONE',  ( 1.000000000000000000, 0.000000000000000000, 0.000000000000000000 ) ) ;
#15085 = CARTESIAN_POINT ( 'NONE',  ( -26.00000000000002132, 10.00000000000000000, -39.99999999999999289 ) ) ;
#15086 = UNCERTAINTY_MEASURE_WITH_UNIT (LENGTH_MEASURE( 1.000000000000000082E-05 ), #10448, 'distance_accuracy_value', 'NONE');
#15087 = ORIENTED_EDGE ( 'NONE', *, *, #2342, .T. ) ;
#15088 = DIRECTION ( 'NONE',  ( 1.000000000000000000, 0.000000000000000000, -0.000000000000000000 ) ) ;
#15089 = FACE_OUTER_BOUND ( 'NONE', #15826, .T. ) ;
#15090 = SURFACE_SIDE_STYLE ('',( #8807 ) ) ;
#15091 = FACE_OUTER_BOUND ( 'NONE', #14704, .T. ) ;
#15093 = EDGE_CURVE ( 'NONE', #14419, #13737, #9801, .T. ) ;
#15092 = CIRCLE ( 'NONE', #11470, 3.300000000000025135 ) ;
#15094 = ADVANCED_FACE ( 'NONE', ( #16112 ), #19163, .T. ) ;
#15095 = CARTESIAN_POINT ( 'NONE',  ( 78.48937290013661539, 80.91625508013694912, -140.0000000000001137 ) ) ;
#15096 = CARTESIAN_POINT ( 'NONE',  ( 0.000000000000000000, 80.91625508013694912, -97.94896630388704750 ) ) ;
#15097 = DIRECTION ( 'NONE',  ( 0.000000000000000000, 1.000000000000000000, 0.000000000000000000 ) ) ;
#15098 = ORIENTED_EDGE ( 'NONE', *, *, #12310, .F. ) ;
#15099 = LINE ( 'NONE', #4186, #17131 ) ;
#15100 = APPLICATION_PROTOCOL_DEFINITION ( 'draft international standard', 'automotive_design', 1998, #18669 ) ;
#15101 = EDGE_LOOP ( 'NONE', ( #4798, #10443, #14153, #20127 ) ) ;
#15102 = PLANE ( 'NONE',  #11926 ) ;
#15103 = VERTEX_POINT ( 'NONE', #19799 ) ;
#15104 = ORIENTED_EDGE ( 'NONE', *, *, #8103, .F. ) ;
#15105 = CIRCLE ( 'NONE', #6224, 10.00000000000000888 ) ;
#15106 = EDGE_LOOP ( 'NONE', ( #7418, #17353, #12533, #12888 ) ) ;
#15107 = CARTESIAN_POINT ( 'NONE',  ( 30.99999999999997513, 10.00000000000000000, 30.99999999999999645 ) ) ;
#15108 = VERTEX_POINT ( 'NONE', #4471 ) ;
#15109 = DIRECTION ( 'NONE',  ( 0.000000000000000000, -0.000000000000000000, -1.000000000000000000 ) ) ;
#15110 = DIRECTION ( 'NONE',  ( -0.000000000000000000, -1.000000000000000000, 0.000000000000000000 ) ) ;
#15111 = ORIENTED_EDGE ( 'NONE', *, *, #11172, .T. ) ;
#15112 = CARTESIAN_POINT ( 'NONE',  ( 0.000000000000000000, 66.00000000000000000, 1.799999999999999600 ) ) ;
#15113 = EDGE_CURVE ( 'NONE', #10510, #15692, #20113, .T. ) ;
#15114 = LINE ( 'NONE', #11924, #18496 ) ;
#15115 = CARTESIAN_POINT ( 'NONE',  ( 463.8334540492693918, 167.8734308960555950, 250.0000000000000000 ) ) ;
#15116 = CARTESIAN_POINT ( 'NONE',  ( 503.8334540492693918, 191.8198460455371333, 71.76606011801538898 ) ) ;
#15117 = AXIS2_PLACEMENT_3D ( 'NONE', #11246, #11563, #13130 ) ;
#15118 = SURFACE_STYLE_USAGE ( .BOTH. , #19430 ) ;
#15119 = VECTOR ( 'NONE', #12393, 1000.000000000000000 ) ;
#15120 =( NAMED_UNIT ( * ) SI_UNIT ( $, .STERADIAN. ) SOLID_ANGLE_UNIT ( ) );
#15121 = CARTESIAN_POINT ( 'NONE',  ( 111.4893729001366012, 125.7247684487574588, 252.0000000000000000 ) ) ;
#15122 =( NAMED_UNIT ( * ) PLANE_ANGLE_UNIT ( ) SI_UNIT ( $, .RADIAN. ) );
#15123 = FACE_OUTER_BOUND ( 'NONE', #19621, .T. ) ;
#15124 =( NAMED_UNIT ( * ) PLANE_ANGLE_UNIT ( ) SI_UNIT ( $, .RADIAN. ) );
#15125 = DIRECTION ( 'NONE',  ( 0.000000000000000000, 0.000000000000000000, -1.000000000000000000 ) ) ;
#15126 = ORIENTED_EDGE ( 'NONE', *, *, #17561, .F. ) ;
#15127 = SURFACE_STYLE_FILL_AREA ( #8749 ) ;
#15128 = EDGE_LOOP ( 'NONE', ( #7629, #6677, #18983, #4089 ) ) ;
#15129 = B_SPLINE_CURVE_WITH_KNOTS ( 'NONE', 3,
 ( #59, #4913, #18622, #14084, #15854, #3367, #12648, #12758, #2944, #13990, #15965, #1809, #17167, #6170 ),
 .UNSPECIFIED., .F., .F.,
 ( 4, 2, 2, 2, 2, 2, 4 ),
 ( 0.000000000000000000, 0.0008478132045734761016, 0.001271719806860251720, 0.001695626409147027447, 0.002119533011433802957, 0.002543439613720578901, 0.003391252818294112140 ),
 .UNSPECIFIED. ) ;
#15130 = ORIENTED_EDGE ( 'NONE', *, *, #14106, .T. ) ;
#15131 = VECTOR ( 'NONE', #1607, 1000.000000000000000 ) ;
#15132 = STYLED_ITEM ( 'NONE', ( #1280 ), #6530 ) ;
#15133 = VERTEX_POINT ( 'NONE', #13544 ) ;
#15134 = AXIS2_PLACEMENT_3D ( 'NONE', #4300, #2848, #7500 ) ;
#15135 = ORIENTED_EDGE ( 'NONE', *, *, #18579, .F. ) ;
#15136 = MANIFOLD_SOLID_BREP ( 'Cut-Extrude1', #3059 ) ;
#15137 = DIRECTION ( 'NONE',  ( -0.000000000000000000, -1.000000000000000000, -0.000000000000000000 ) ) ;
#15138 = LINE ( 'NONE', #10190, #6612 ) ;
#15139 = DIRECTION ( 'NONE',  ( 0.000000000000000000, 1.000000000000000000, 0.000000000000000000 ) ) ;
#15140 = ADVANCED_FACE ( 'NONE', ( #12188 ), #857, .F. ) ;
#15141 = SURFACE_STYLE_FILL_AREA ( #18113 ) ;
#15142 = DIRECTION ( 'NONE',  ( 0.000000000000000000, 0.000000000000000000, -1.000000000000000000 ) ) ;
#15143 = PRESENTATION_LAYER_ASSIGNMENT (  '', '', ( #11857 ) ) ;
#15144 = CARTESIAN_POINT ( 'NONE',  ( 6.299999999999999822, 0.000000000000000000, 0.000000000000000000 ) ) ;
#15145 = SURFACE_STYLE_FILL_AREA ( #4321 ) ;
#15146 = AXIS2_PLACEMENT_3D ( 'NONE', #10377, #5634, #7291 ) ;
#15147 = VECTOR ( 'NONE', #15502, 1000.000000000000000 ) ;
#15148 = ADVANCED_FACE ( 'NONE', ( #8708 ), #5912, .F. ) ;
#15149 = EDGE_CURVE ( 'NONE', #12573, #8577, #5605, .T. ) ;
#15150 = ORIENTED_EDGE ( 'NONE', *, *, #6858, .T. ) ;
#15151 = EDGE_LOOP ( 'NONE', ( #13271, #19293, #16351, #11373, #8821, #13346 ) ) ;
#15152 = EDGE_LOOP ( 'NONE', ( #15347, #13455, #9008, #10555 ) ) ;
#15153 = CARTESIAN_POINT ( 'NONE',  ( -58.16843972078500258, 319.7545334744432353, 485.1700099148404206 ) ) ;
#15154 = EDGE_LOOP ( 'NONE', ( #868, #12607, #2190, #2311 ) ) ;
#15155 = ORIENTED_EDGE ( 'NONE', *, *, #13783, .F. ) ;
#15156 = CARTESIAN_POINT ( 'NONE',  ( 35.99999999999999289, 8.000000000000000000, 21.99999999999999645 ) ) ;
#15157 = AXIS2_PLACEMENT_3D ( 'NONE', #13894, #79, #9366 ) ;
#15158 = AXIS2_PLACEMENT_3D ( 'NONE', #6852, #9723, #542 ) ;
#15159 = DIRECTION ( 'NONE',  ( 0.000000000000000000, 0.000000000000000000, -1.000000000000000000 ) ) ;
#15160 = DIRECTION ( 'NONE',  ( -6.120180426682197225E-17, 0.6235460666509320404, -0.7817866094812263578 ) ) ;
#15161 = EDGE_CURVE ( 'NONE', #10815, #11484, #10350, .T. ) ;
#15162 = SURFACE_STYLE_FILL_AREA ( #18038 ) ;
#15164 = ADVANCED_FACE ( 'NONE', ( #15091 ), #940, .T. ) ;
#15163 = DIRECTION ( 'NONE',  ( -0.000000000000000000, -1.000000000000000000, -0.000000000000000000 ) ) ;
#15165 = AXIS2_PLACEMENT_3D ( 'NONE', #13712, #2357, #5879 ) ;
#15166 = FILL_AREA_STYLE ('',( #8416 ) ) ;
#15167 = DIRECTION ( 'NONE',  ( 0.000000000000000000, -2.352167425053297897E-16, -1.000000000000000000 ) ) ;
#15168 = DIRECTION ( 'NONE',  ( -1.000000000000000000, -9.815121534730717399E-17, 0.000000000000000000 ) ) ;
#15169 = CARTESIAN_POINT ( 'NONE',  ( -81.18192946989111647, 216.7545334744432921, 489.5655098179833544 ) ) ;
#15170 = FILL_AREA_STYLE_COLOUR ( '', #20240 ) ;
#15171 = EDGE_CURVE ( 'NONE', #8912, #5141, #6435, .T. ) ;
#15172 = EDGE_LOOP ( 'NONE', ( #20333, #5251, #7598, #13288 ) ) ;
#15173 = DIRECTION ( 'NONE',  ( 0.000000000000000000, 1.000000000000000000, 0.000000000000000000 ) ) ;
#15174 = FILL_AREA_STYLE ('',( #9285 ) ) ;
#15175 = CARTESIAN_POINT ( 'NONE',  ( 463.8334540492693350, 214.2156642432025251, 250.0000000000000000 ) ) ;
#15176 = AXIS2_PLACEMENT_3D ( 'NONE', #16957, #7779, #14060 ) ;
#15177 = EDGE_CURVE ( 'NONE', #6967, #13170, #12025, .T. ) ;
#15178 = CIRCLE ( 'NONE', #3311, 36.50000000000000000 ) ;
#15179 = EDGE_CURVE ( 'NONE', #1776, #12056, #10362, .T. ) ;
#15180 = VERTEX_POINT ( 'NONE', #15613 ) ;
#15181 = EDGE_CURVE ( 'NONE', #7061, #7067, #1646, .T. ) ;
#15182 = ORIENTED_EDGE ( 'NONE', *, *, #20178, .F. ) ;
#15183 = DIRECTION ( 'NONE',  ( 1.000000000000000000, 9.815121534730717399E-17, 0.000000000000000000 ) ) ;
#15184 = CARTESIAN_POINT ( 'NONE',  ( -31.00000000000000000, 8.000000000000000000, 30.99999999999999289 ) ) ;
#15185 = EDGE_LOOP ( 'NONE', ( #19446, #12182, #9940, #10630 ) ) ;
#15186 = CIRCLE ( 'NONE', #1320, 12.00000000000000178 ) ;
#15187 =( NAMED_UNIT ( * ) SI_UNIT ( $, .STERADIAN. ) SOLID_ANGLE_UNIT ( ) );
#15189 = EDGE_CURVE ( 'NONE', #6242, #12591, #10850, .T. ) ;
#15188 =( NAMED_UNIT ( * ) PLANE_ANGLE_UNIT ( ) SI_UNIT ( $, .RADIAN. ) );
#15190 = CARTESIAN_POINT ( 'NONE',  ( -80.91178762245726830, 140.4048636633015690, 500.8237260975782874 ) ) ;
#15191 = SURFACE_STYLE_USAGE ( .BOTH. , #10649 ) ;
#15192 = FACE_OUTER_BOUND ( 'NONE', #8529, .T. ) ;
#15193 = ORIENTED_EDGE ( 'NONE', *, *, #10779, .F. ) ;
#15194 = DIRECTION ( 'NONE',  ( 0.000000000000000000, -1.000000000000000000, 0.000000000000000000 ) ) ;
#15195 = LINE ( 'NONE', #7275, #1075 ) ;
#15196 = DIRECTION ( 'NONE',  ( 1.000000000000000000, 0.000000000000000000, 0.000000000000000000 ) ) ;
#15197 = ORIENTED_EDGE ( 'NONE', *, *, #5960, .F. ) ;
#15198 = ORIENTED_EDGE ( 'NONE', *, *, #15949, .F. ) ;
#15199 = CARTESIAN_POINT ( 'NONE',  ( 4.549999999999999822, 0.000000000000000000, -14.27500000000000036 ) ) ;
#15200 = ADVANCED_FACE ( 'NONE', ( #11063 ), #7858, .F. ) ;
#15201 = VERTEX_POINT ( 'NONE', #8075 ) ;
#15202 = VECTOR ( 'NONE', #8506, 1000.000000000000000 ) ;
#15203 = ORIENTED_EDGE ( 'NONE', *, *, #10924, .T. ) ;
#15204 = MANIFOLD_SOLID_BREP ( 'Boss-Extrude1', #8017 ) ;
#15205 = CIRCLE ( 'NONE', #19134, 10.00000000000000888 ) ;
#15206 = ORIENTED_EDGE ( 'NONE', *, *, #5756, .F. ) ;
#15207 = EDGE_CURVE ( 'NONE', #16622, #625, #18973, .T. ) ;
#15208 = LINE ( 'NONE', #7575, #7112 ) ;
#15209 = ORIENTED_EDGE ( 'NONE', *, *, #4740, .T. ) ;
#15210 = FACE_OUTER_BOUND ( 'NONE', #5188, .T. ) ;
#15211 = PLANE ( 'NONE',  #10660 ) ;
#15212 = DIRECTION ( 'NONE',  ( -1.000000000000000000, -0.000000000000000000, -0.000000000000000000 ) ) ;
#15213 = PLANE ( 'NONE',  #84 ) ;
#15214 = PRESENTATION_STYLE_ASSIGNMENT (( #3031 ) ) ;
#15215 = VECTOR ( 'NONE', #14204, 1000.000000000000000 ) ;
#15216 = CIRCLE ( 'NONE', #14224, 2.000000000000001776 ) ;
#15217 = CARTESIAN_POINT ( 'NONE',  ( -26.00000000000002132, 10.00000000000000000, -31.00000000000003553 ) ) ;
#15218 = CARTESIAN_POINT ( 'NONE',  ( 26.00000000000001066, 68.00000000000000000, -31.00000000000002487 ) ) ;
#15219 =( GEOMETRIC_REPRESENTATION_CONTEXT ( 3 ) GLOBAL_UNCERTAINTY_ASSIGNED_CONTEXT ( ( #2699 ) ) GLOBAL_UNIT_ASSIGNED_CONTEXT ( ( #8225, #19335, #11513 ) ) REPRESENTATION_CONTEXT ( 'NONE', 'WORKASPACE' ) );
#15220 = EDGE_CURVE ( 'NONE', #5238, #13110, #12501, .T. ) ;
#15221 = CARTESIAN_POINT ( 'NONE',  ( 475.8334540492694487, 134.2156642432025251, 245.0000000000000000 ) ) ;
#15222 = CARTESIAN_POINT ( 'NONE',  ( -34.99999999999998579, 3.000000000000000000, 18.50000000000000355 ) ) ;
#15223 = CARTESIAN_POINT ( 'NONE',  ( -20.00000000000003197, 0.000000000000000000, 37.00000000000000711 ) ) ;
#15224 =( NAMED_UNIT ( * ) SI_UNIT ( $, .STERADIAN. ) SOLID_ANGLE_UNIT ( ) );
#15225 = CARTESIAN_POINT ( 'NONE',  ( -118.0000000000000284, 316.7545334744432921, 205.1946179577815883 ) ) ;
#15226 = AXIS2_PLACEMENT_3D ( 'NONE', #4299, #10787, #9037 ) ;
#15227 = PRESENTATION_STYLE_ASSIGNMENT (( #13687 ) ) ;
#15228 = VECTOR ( 'NONE', #8134, 1000.000000000000000 ) ;
#15229 = DIRECTION ( 'NONE',  ( -0.000000000000000000, -0.000000000000000000, 1.000000000000000000 ) ) ;
#15230 = VECTOR ( 'NONE', #17414, 1000.000000000000000 ) ;
#15231 = CARTESIAN_POINT ( 'NONE',  ( -33.00000000000000000, 8.000000000000000000, -22.00000000000000355 ) ) ;
#15232 = ORIENTED_EDGE ( 'NONE', *, *, #13450, .T. ) ;
#15233 = EDGE_LOOP ( 'NONE', ( #13516, #19784, #9316, #11266, #3215 ) ) ;
#15234 = AXIS2_PLACEMENT_3D ( 'NONE', #7698, #15435, #20146 ) ;
#15235 = UNCERTAINTY_MEASURE_WITH_UNIT (LENGTH_MEASURE( 1.000000000000000082E-05 ), #2718, 'distance_accuracy_value', 'NONE');
#15236 = ORIENTED_EDGE ( 'NONE', *, *, #18786, .T. ) ;
#15237 = AXIS2_PLACEMENT_3D ( 'NONE', #11487, #3663, #8413 ) ;
#15238 = VERTEX_POINT ( 'NONE', #7660 ) ;
#15239 = DIRECTION ( 'NONE',  ( 0.000000000000000000, 0.000000000000000000, -1.000000000000000000 ) ) ;
#15240 = ORIENTED_EDGE ( 'NONE', *, *, #14684, .F. ) ;
#15241 = DIRECTION ( 'NONE',  ( -0.000000000000000000, 1.000000000000000000, -0.000000000000000000 ) ) ;
#15242 =( LENGTH_UNIT ( ) NAMED_UNIT ( * ) SI_UNIT ( .MILLI., .METRE. ) );
#15243 = PRODUCT_DEFINITION_FORMATION_WITH_SPECIFIED_SOURCE ( 'ANY', '', #16206, .NOT_KNOWN. ) ;
#15244 = DIRECTION ( 'NONE',  ( 0.000000000000000000, 0.000000000000000000, 1.000000000000000000 ) ) ;
#15245 = VECTOR ( 'NONE', #10733, 1000.000000000000000 ) ;
#15246 = DIRECTION ( 'NONE',  ( -3.328238341717372086E-14, 0.000000000000000000, 1.000000000000000000 ) ) ;
#15247 = FACE_OUTER_BOUND ( 'NONE', #15574, .T. ) ;
#15248 = DIRECTION ( 'NONE',  ( 1.000000000000000000, 0.000000000000000000, 0.000000000000000000 ) ) ;
#15249 = FILL_AREA_STYLE ('',( #13502 ) ) ;
#15250 = SURFACE_STYLE_FILL_AREA ( #5875 ) ;
#15251 = CIRCLE ( 'NONE', #13932, 3.300000000000004263 ) ;
#15252 = VECTOR ( 'NONE', #19051, 1000.000000000000000 ) ;
#15253 = DIRECTION ( 'NONE',  ( -0.000000000000000000, -1.000000000000000000, -0.000000000000000000 ) ) ;
#15254 = DIRECTION ( 'NONE',  ( -1.000000000000000000, 0.000000000000000000, -5.551115123125777653E-14 ) ) ;
#15255 = EDGE_CURVE ( 'NONE', #19144, #1021, #10046, .T. ) ;
#15256 = AXIS2_PLACEMENT_3D ( 'NONE', #15049, #1867, #11959 ) ;
#15257 = VERTEX_POINT ( 'NONE', #15915 ) ;
#15258 = ORIENTED_EDGE ( 'NONE', *, *, #6657, .F. ) ;
#15259 = CARTESIAN_POINT ( 'NONE',  ( 31.00000000000001776, 0.000000000000000000, -19.99999999999991473 ) ) ;
#15260 = EDGE_LOOP ( 'NONE', ( #15298, #6439, #9856, #2979, #1409, #15580 ) ) ;
#15261 = VERTEX_POINT ( 'NONE', #7960 ) ;
#15262 = CIRCLE ( 'NONE', #6386, 10.00000000000000178 ) ;
#15263 = CIRCLE ( 'NONE', #17226, 3.300000000000000711 ) ;
#15264 = AXIS2_PLACEMENT_3D ( 'NONE', #6301, #9572, #14332 ) ;
#15265 = UNCERTAINTY_MEASURE_WITH_UNIT (LENGTH_MEASURE( 1.000000000000000082E-05 ), #2905, 'distance_accuracy_value', 'NONE');
#15266 = DIRECTION ( 'NONE',  ( -1.000000000000000000, 0.000000000000000000, 0.000000000000000000 ) ) ;
#15267 =( LENGTH_UNIT ( ) NAMED_UNIT ( * ) SI_UNIT ( .MILLI., .METRE. ) );
#15268 = LINE ( 'NONE', #5682, #17925 ) ;
#15269 = STYLED_ITEM ( 'NONE', ( #20003 ), #1329 ) ;
#15270 = CARTESIAN_POINT ( 'NONE',  ( 406.3334540492693350, 242.8734308960556234, 250.0000000000000000 ) ) ;
#15271 = COLOUR_RGB ( '', 0.08235294, 0.09019608, 0.10196078) ;
#15272 = CARTESIAN_POINT ( 'NONE',  ( -1.450371633464477160E-15, 216.7545334744432921, 509.3921618609452935 ) ) ;
#15273 = ADVANCED_FACE ( 'NONE', ( #9301 ), #1758, .T. ) ;
#15274 = DIRECTION ( 'NONE',  ( 1.000000000000000000, -0.000000000000000000, -0.000000000000000000 ) ) ;
#15275 = MANIFOLD_SOLID_BREP ( 'Boss-Extrude4', #12277 ) ;
#15276 = DIRECTION ( 'NONE',  ( 0.000000000000000000, 0.000000000000000000, 1.000000000000000000 ) ) ;
#15277 = CARTESIAN_POINT ( 'NONE',  ( -80.86756541979772805, 139.7703989356676004, 489.5655098179837523 ) ) ;
#15278 = DIRECTION ( 'NONE',  ( 1.000000000000000000, 9.815121534730717399E-17, 0.000000000000000000 ) ) ;
#15279 = ORIENTED_EDGE ( 'NONE', *, *, #6624, .F. ) ;
#15280 =( LENGTH_UNIT ( ) NAMED_UNIT ( * ) SI_UNIT ( .MILLI., .METRE. ) );
#15281 = ADVANCED_BREP_SHAPE_REPRESENTATION ( '', ( #8230, #15010, #15275, #8135, #2741 ), #14604 ) ;
#15282 = AXIS2_PLACEMENT_3D ( 'NONE', #11161, #238, #131 ) ;
#15283 = VECTOR ( 'NONE', #12007, 1000.000000000000000 ) ;
#15284 = COLOUR_RGB ( '', 0.66274510, 0.83137255, 0.94901961) ;
#15285 = STYLED_ITEM ( 'NONE', ( #12719 ), #1368 ) ;
#15286 = ADVANCED_FACE ( 'NONE', ( #11426 ), #589, .F. ) ;
#15287 = AXIS2_PLACEMENT_3D ( 'NONE', #3612, #5169, #6823 ) ;
#15288 = ORIENTED_EDGE ( 'NONE', *, *, #17534, .T. ) ;
#15289 = UNCERTAINTY_MEASURE_WITH_UNIT (LENGTH_MEASURE( 1.000000000000000082E-05 ), #4292, 'distance_accuracy_value', 'NONE');
#15290 = ADVANCED_FACE ( 'NONE', ( #5246 ), #3694, .T. ) ;
#15291 = ORIENTED_EDGE ( 'NONE', *, *, #20299, .F. ) ;
#15292 = MECHANICAL_DESIGN_GEOMETRIC_PRESENTATION_REPRESENTATION (  '', ( #8697 ), #13321 ) ;
#15293 = LINE ( 'NONE', #1325, #10022 ) ;
#15294 =( GEOMETRIC_REPRESENTATION_CONTEXT ( 3 ) GLOBAL_UNCERTAINTY_ASSIGNED_CONTEXT ( ( #19982 ) ) GLOBAL_UNIT_ASSIGNED_CONTEXT ( ( #8059, #10945, #10740 ) ) REPRESENTATION_CONTEXT ( 'NONE', 'WORKASPACE' ) );
#15295 = DIRECTION ( 'NONE',  ( -0.000000000000000000, -0.000000000000000000, 1.000000000000000000 ) ) ;
#15296 = UNCERTAINTY_MEASURE_WITH_UNIT (LENGTH_MEASURE( 1.000000000000000082E-05 ), #15887, 'distance_accuracy_value', 'NONE');
#15297 = AXIS2_PLACEMENT_3D ( 'NONE', #13437, #15274, #1120 ) ;
#15298 = ORIENTED_EDGE ( 'NONE', *, *, #19949, .F. ) ;
#15299 = DIRECTION ( 'NONE',  ( -0.000000000000000000, -0.000000000000000000, -1.000000000000000000 ) ) ;
#15300 = FILL_AREA_STYLE ('',( #13457 ) ) ;
#15301 = EDGE_CURVE ( 'NONE', #12228, #7675, #5158, .T. ) ;
#15302 = CARTESIAN_POINT ( 'NONE',  ( 31.00000000000001776, 0.000000000000000000, -25.99999999999999645 ) ) ;
#15303 = FILL_AREA_STYLE ('',( #13548 ) ) ;
#15304 = CIRCLE ( 'NONE', #5099, 4.999999999999997335 ) ;
#15305 = EDGE_LOOP ( 'NONE', ( #11239, #19148 ) ) ;
#15306 = ADVANCED_FACE ( 'NONE', ( #2133 ), #379, .F. ) ;
#15307 = DIRECTION ( 'NONE',  ( 0.000000000000000000, -0.7071067811865336949, -0.7071067811865614505 ) ) ;
#15308 = CARTESIAN_POINT ( 'NONE',  ( -21.85283368562565443, 317.7545334744432353, 481.2863735482146694 ) ) ;
#15309 = APPLICATION_PROTOCOL_DEFINITION ( 'draft international standard', 'automotive_design', 1998, #8815 ) ;
#15310 = ORIENTED_EDGE ( 'NONE', *, *, #19947, .F. ) ;
#15311 = ORIENTED_EDGE ( 'NONE', *, *, #1946, .T. ) ;
#15312 = FILL_AREA_STYLE_COLOUR ( '', #5667 ) ;
#15313 = AXIS2_PLACEMENT_3D ( 'NONE', #19078, #332, #12930 ) ;
#15314 = ORIENTED_EDGE ( 'NONE', *, *, #14677, .T. ) ;
#15315 = VECTOR ( 'NONE', #4782, 1000.000000000000000 ) ;
#15316 = VERTEX_POINT ( 'NONE', #16390 ) ;
#15317 = AXIS2_PLACEMENT_3D ( 'NONE', #3914, #12436, #14836 ) ;
#15318 = EDGE_CURVE ( 'NONE', #12661, #6513, #17705, .T. ) ;
#15319 = ORIENTED_EDGE ( 'NONE', *, *, #13237, .T. ) ;
#15320 = VECTOR ( 'NONE', #19060, 1000.000000000000000 ) ;
#15321 = PLANE ( 'NONE',  #18921 ) ;
#15322 = ORIENTED_EDGE ( 'NONE', *, *, #2838, .F. ) ;
#15323 = CARTESIAN_POINT ( 'NONE',  ( 0.4453342799582463707, 140.5544088492690946, 500.9879276894058080 ) ) ;
#15324 = VECTOR ( 'NONE', #19822, 1000.000000000000000 ) ;
#15325 = EDGE_LOOP ( 'NONE', ( #15631, #581 ) ) ;
#15326 = EDGE_CURVE ( 'NONE', #1696, #16787, #2224, .T. ) ;
#15327 = LINE ( 'NONE', #4201, #11252 ) ;
#15328 = DIRECTION ( 'NONE',  ( -0.000000000000000000, 1.000000000000000000, -0.000000000000000000 ) ) ;
#15329 = FILL_AREA_STYLE ('',( #12039 ) ) ;
#15330 = CARTESIAN_POINT ( 'NONE',  ( -31.00000000000000000, 19.00000000000000000, 30.99999999999999289 ) ) ;
#15331 =( NAMED_UNIT ( * ) SI_UNIT ( $, .STERADIAN. ) SOLID_ANGLE_UNIT ( ) );
#15332 = COLOUR_RGB ( '', 0.09019608, 0.27058824, 0.51372549) ;
#15333 = FACE_OUTER_BOUND ( 'NONE', #2825, .T. ) ;
#15334 = CARTESIAN_POINT ( 'NONE',  ( 30.99999999999996092, 3.000000000000000000, -30.99999999999999289 ) ) ;
#15335 = CARTESIAN_POINT ( 'NONE',  ( 463.8334540492693350, 191.8198460455371333, 235.0057801310552463 ) ) ;
#15336 = CARTESIAN_POINT ( 'NONE',  ( 21.99999999999998224, 10.00000000000000000, -35.99999999999999289 ) ) ;
#15337 = DIRECTION ( 'NONE',  ( -3.553708640349232828E-17, 1.000000000000000000, 4.699395265751666769E-17 ) ) ;
#15338 =( NAMED_UNIT ( * ) SI_UNIT ( $, .STERADIAN. ) SOLID_ANGLE_UNIT ( ) );
#15339 =( LENGTH_UNIT ( ) NAMED_UNIT ( * ) SI_UNIT ( .MILLI., .METRE. ) );
#15340 = AXIS2_PLACEMENT_3D ( 'NONE', #7769, #3006, #12599 ) ;
#15341 = SURFACE_STYLE_USAGE ( .BOTH. , #12340 ) ;
#15342 = FILL_AREA_STYLE ('',( #2443 ) ) ;
#15343 = CARTESIAN_POINT ( 'NONE',  ( 0.000000000000000000, 167.9162550801369491, 0.000000000000000000 ) ) ;
#15344 = ORIENTED_EDGE ( 'NONE', *, *, #1817, .F. ) ;
#15345 = AXIS2_PLACEMENT_3D ( 'NONE', #7738, #7443, #3090 ) ;
#15346 = EDGE_LOOP ( 'NONE', ( #6123, #14725, #12492, #12994 ) ) ;
#15347 = ORIENTED_EDGE ( 'NONE', *, *, #9151, .F. ) ;
#15349 = ORIENTED_EDGE ( 'NONE', *, *, #4220, .F. ) ;
#15348 = ADVANCED_FACE ( 'NONE', ( #14811 ), #16289, .F. ) ;
#15350 = CARTESIAN_POINT ( 'NONE',  ( -79.62203884913070340, 138.8314538163270981, 489.8899081770637167 ) ) ;
#15351 = VERTEX_POINT ( 'NONE', #18000 ) ;
#15352 = CIRCLE ( 'NONE', #9094, 17.52499999999999858 ) ;
#15353 = LINE ( 'NONE', #1276, #17910 ) ;
#15354 = FACE_OUTER_BOUND ( 'NONE', #10282, .T. ) ;
#15355 = DIRECTION ( 'NONE',  ( 0.000000000000000000, 0.000000000000000000, -1.000000000000000000 ) ) ;
#15356 = ORIENTED_EDGE ( 'NONE', *, *, #9612, .F. ) ;
#15357 = ADVANCED_FACE ( 'NONE', ( #15992, #283 ), #881, .T. ) ;
#15358 =( NAMED_UNIT ( * ) PLANE_ANGLE_UNIT ( ) SI_UNIT ( $, .RADIAN. ) );
#15359 = VECTOR ( 'NONE', #4949, 1000.000000000000000 ) ;
#15360 = FACE_OUTER_BOUND ( 'NONE', #9216, .T. ) ;
#15361 = CARTESIAN_POINT ( 'NONE',  ( -23.00000000000002487, 10.00000000000000000, -36.99999999999999289 ) ) ;
#15362 = DIRECTION ( 'NONE',  ( -1.000000000000000000, 0.000000000000000000, 0.000000000000000000 ) ) ;
#15363 = CARTESIAN_POINT ( 'NONE',  ( 25.99999999999998224, 10.00000000000000000, -31.00000000000003197 ) ) ;
#15364 = LINE ( 'NONE', #4529, #3742 ) ;
#15365 = SURFACE_SIDE_STYLE ('',( #20175 ) ) ;
#15366 = CIRCLE ( 'NONE', #20286, 3.300000000000011369 ) ;
#15367 = ORIENTED_EDGE ( 'NONE', *, *, #8426, .T. ) ;
#15368 = VERTEX_POINT ( 'NONE', #2540 ) ;
#15369 = FILL_AREA_STYLE_COLOUR ( '', #2768 ) ;
#15370 = ORIENTED_EDGE ( 'NONE', *, *, #18695, .T. ) ;
#15371 = ORIENTED_EDGE ( 'NONE', *, *, #17823, .T. ) ;
#15372 =( NAMED_UNIT ( * ) SI_UNIT ( $, .STERADIAN. ) SOLID_ANGLE_UNIT ( ) );
#15373 = ORIENTED_EDGE ( 'NONE', *, *, #5575, .F. ) ;
#15374 = CARTESIAN_POINT ( 'NONE',  ( -44.50085094405407915, 175.4489062796178871, 505.3921618609452935 ) ) ;
#15375 = DIRECTION ( 'NONE',  ( -0.000000000000000000, 1.000000000000000000, -0.000000000000000000 ) ) ;
#15376 =( LENGTH_UNIT ( ) NAMED_UNIT ( * ) SI_UNIT ( .MILLI., .METRE. ) );
#15377 = FILL_AREA_STYLE_COLOUR ( '', #841 ) ;
#15378 = SURFACE_STYLE_FILL_AREA ( #7239 ) ;
#15379 = ADVANCED_FACE ( 'NONE', ( #7400 ), #12046, .F. ) ;
#15380 = CARTESIAN_POINT ( 'NONE',  ( 458.8334540492693350, 242.8734308960556234, 0.000000000000000000 ) ) ;
#15381 = CARTESIAN_POINT ( 'NONE',  ( 19.99999999999995381, 3.000000000000000000, -36.99999999999999289 ) ) ;
#15382 = FACE_OUTER_BOUND ( 'NONE', #18989, .T. ) ;
#15383 = MANIFOLD_SOLID_BREP ( 'Cut-Extrude4[1]', #13298 ) ;
#15384 = CYLINDRICAL_SURFACE ( 'NONE', #8961, 8.000000000000000000 ) ;
#15385 = CARTESIAN_POINT ( 'NONE',  ( -22.00000000000001776, 6.000000000000000000, 32.00000000000000711 ) ) ;
#15386 = ORIENTED_EDGE ( 'NONE', *, *, #12398, .F. ) ;
#15387 = SURFACE_STYLE_FILL_AREA ( #11986 ) ;
#15388 = DIRECTION ( 'NONE',  ( 0.000000000000000000, -1.000000000000000000, 0.000000000000000000 ) ) ;
#15389 = LINE ( 'NONE', #11988, #9342 ) ;
#15390 = ORIENTED_EDGE ( 'NONE', *, *, #14555, .F. ) ;
#15391 = EDGE_CURVE ( 'NONE', #14706, #20158, #2475, .T. ) ;
#15392 = EDGE_LOOP ( 'NONE', ( #17787, #19001, #9319, #11057 ) ) ;
#15393 = CARTESIAN_POINT ( 'NONE',  ( 0.000000000000000000, 376.0487089519837127, -155.0000000000033253 ) ) ;
#15394 = FACE_OUTER_BOUND ( 'NONE', #9262, .T. ) ;
#15395 = ORIENTED_EDGE ( 'NONE', *, *, #17823, .F. ) ;
#15396 = CARTESIAN_POINT ( 'NONE',  ( 31.00000000000003553, 19.00000000000000000, 20.99999999999999289 ) ) ;
#15397 = CARTESIAN_POINT ( 'NONE',  ( -79.19244403447679304, 140.1600456049978618, 501.4957876295819119 ) ) ;
#15398 = CARTESIAN_POINT ( 'NONE',  ( 1.574999999999999956, -14.92500000000000071, -1.827785347727424768E-15 ) ) ;
#15399 = VECTOR ( 'NONE', #3227, 1000.000000000000000 ) ;
#15400 = DIRECTION ( 'NONE',  ( 1.000000000000000000, 0.000000000000000000, 0.000000000000000000 ) ) ;
#15401 = CARTESIAN_POINT ( 'NONE',  ( -64.99999999999995737, 317.7545334744432353, 495.1946179577816451 ) ) ;
#15402 = EDGE_CURVE ( 'NONE', #6120, #4513, #19730, .T. ) ;
#15403 = LINE ( 'NONE', #1232, #13339 ) ;
#15404 = VECTOR ( 'NONE', #1828, 1000.000000000000000 ) ;
#15405 = EDGE_LOOP ( 'NONE', ( #674, #14256, #13624, #4891 ) ) ;
#15406 = DIRECTION ( 'NONE',  ( 0.000000000000000000, 0.000000000000000000, 1.000000000000000000 ) ) ;
#15407 = CARTESIAN_POINT ( 'NONE',  ( 153.4893729001366580, 145.9162550801369491, 250.0000000000000000 ) ) ;
#15408 = PLANE ( 'NONE',  #3088 ) ;
#15409 = APPLICATION_PROTOCOL_DEFINITION ( 'draft international standard', 'automotive_design', 1998, #2078 ) ;
#15410 = ORIENTED_EDGE ( 'NONE', *, *, #5741, .T. ) ;
#15411 = ORIENTED_EDGE ( 'NONE', *, *, #16009, .F. ) ;
#15412 = PRODUCT_DEFINITION ( 'UNKNOWN', '', #3044, #8636 ) ;
#15413 = CARTESIAN_POINT ( 'NONE',  ( 30.99999999999999645, 0.000000000000000000, 26.00000000000000355 ) ) ;
#15414 = ORIENTED_EDGE ( 'NONE', *, *, #4335, .F. ) ;
#15415 = EDGE_LOOP ( 'NONE', ( #4310, #12742, #13449, #17137, #12862, #2368, #5013, #16945 ) ) ;
#15416 = ORIENTED_EDGE ( 'NONE', *, *, #14754, .T. ) ;
#15417 = EDGE_CURVE ( 'NONE', #6058, #7572, #14991, .T. ) ;
#15418 = LINE ( 'NONE', #4194, #3483 ) ;
#15419 = ORIENTED_EDGE ( 'NONE', *, *, #10008, .F. ) ;
#15420 = EDGE_CURVE ( 'NONE', #1728, #2022, #13577, .T. ) ;
#15421 = DIRECTION ( 'NONE',  ( -1.000000000000000000, -0.000000000000000000, 3.854941057726247958E-16 ) ) ;
#15422 =( LENGTH_UNIT ( ) NAMED_UNIT ( * ) SI_UNIT ( .MILLI., .METRE. ) );
#15423 = SURFACE_STYLE_USAGE ( .BOTH. , #5933 ) ;
#15424 = DIRECTION ( 'NONE',  ( -1.000000000000000000, 0.000000000000000000, 0.000000000000000000 ) ) ;
#15425 = SURFACE_SIDE_STYLE ('',( #13765 ) ) ;
#15426 = PLANE ( 'NONE',  #1807 ) ;
#15427 = CARTESIAN_POINT ( 'NONE',  ( -80.99999999999995737, 138.7545334744432637, 501.8237260975782874 ) ) ;
#15428 = ADVANCED_FACE ( 'NONE', ( #784 ), #5541, .F. ) ;
#15429 = CARTESIAN_POINT ( 'NONE',  ( 0.000000000000000000, 0.000000000000000000, 0.000000000000000000 ) ) ;
#15430 = DIRECTION ( 'NONE',  ( 1.000000000000000000, 0.000000000000000000, 0.000000000000000000 ) ) ;
#15431 = FACE_OUTER_BOUND ( 'NONE', #11918, .T. ) ;
#15432 = LINE ( 'NONE', #7695, #9312 ) ;
#15433 =( NAMED_UNIT ( * ) PLANE_ANGLE_UNIT ( ) SI_UNIT ( $, .RADIAN. ) );
#15434 = SURFACE_STYLE_FILL_AREA ( #1688 ) ;
#15435 = DIRECTION ( 'NONE',  ( 1.000000000000000000, 0.000000000000000000, 0.000000000000000000 ) ) ;
#15436 = DIRECTION ( 'NONE',  ( -0.000000000000000000, -1.000000000000000000, 0.000000000000000000 ) ) ;
#15437 = EDGE_CURVE ( 'NONE', #8671, #17668, #3993, .T. ) ;
#15438 = CARTESIAN_POINT ( 'NONE',  ( 0.000000000000000000, 381.0487089519832011, -80.00000000000332534 ) ) ;
#15439 = EDGE_CURVE ( 'NONE', #9081, #10510, #13987, .T. ) ;
#15440 = ORIENTED_EDGE ( 'NONE', *, *, #11994, .T. ) ;
#15441 = ADVANCED_FACE ( 'NONE', ( #9231 ), #6166, .T. ) ;
#15442 = ORIENTED_EDGE ( 'NONE', *, *, #8300, .T. ) ;
#15443 = ORIENTED_EDGE ( 'NONE', *, *, #15318, .F. ) ;
#15444 = CARTESIAN_POINT ( 'NONE',  ( -58.16843972078500258, 317.7545334744432353, 485.1700099148404206 ) ) ;
#15445 = EDGE_CURVE ( 'NONE', #19684, #17548, #7100, .T. ) ;
#15446 = DIRECTION ( 'NONE',  ( 0.000000000000000000, 0.000000000000000000, 1.000000000000000000 ) ) ;
#15447 = ORIENTED_EDGE ( 'NONE', *, *, #13775, .T. ) ;
#15448 = PRESENTATION_LAYER_ASSIGNMENT (  '', '', ( #5612 ) ) ;
#15449 = CARTESIAN_POINT ( 'NONE',  ( 1.574999999999999956, 14.92500000000000071, 0.000000000000000000 ) ) ;
#15450 = SURFACE_SIDE_STYLE ('',( #12841 ) ) ;
#15451 = AXIS2_PLACEMENT_3D ( 'NONE', #17114, #6487, #1831 ) ;
#15452 = EDGE_LOOP ( 'NONE', ( #10346, #13512, #15554, #17990, #2445, #20077 ) ) ;
#15453 = SURFACE_STYLE_FILL_AREA ( #17004 ) ;
#15454 = B_SPLINE_CURVE_WITH_KNOTS ( 'NONE', 3,
 ( #20250, #9217, #9021, #16866, #6153, #15323, #18697, #15530, #10669, #4588, #1351, #8828, #10872, #13565 ),
 .UNSPECIFIED., .F., .F.,
 ( 4, 2, 2, 2, 2, 2, 4 ),
 ( 0.000000000000000000, 0.0002607493764501894956, 0.0005214987529003789913, 0.0007822481293505684869, 0.001042997505800757983, 0.001564496258701136974, 0.002085995011601515965 ),
 .UNSPECIFIED. ) ;
#15455 = CARTESIAN_POINT ( 'NONE',  ( -1.450371633464476962E-15, 138.7545334744432637, 509.3921618609452935 ) ) ;
#15456 = CARTESIAN_POINT ( 'NONE',  ( -9.162750170181086975E-15, 142.0976792249508946, 485.4122383872432351 ) ) ;
#15457 = EDGE_CURVE ( 'NONE', #4282, #17048, #20145, .T. ) ;
#15458 = CARTESIAN_POINT ( 'NONE',  ( 26.00000000000000000, 11.00000000000000000, 31.00000000000003197 ) ) ;
#15459 = CYLINDRICAL_SURFACE ( 'NONE', #18855, 10.00000000000000888 ) ;
#15460 = SURFACE_STYLE_FILL_AREA ( #18826 ) ;
#15461 = CARTESIAN_POINT ( 'NONE',  ( -82.18192946989243808, 138.7545334744432637, 490.5655098179832976 ) ) ;
#15462 =( NAMED_UNIT ( * ) PLANE_ANGLE_UNIT ( ) SI_UNIT ( $, .RADIAN. ) );
#15463 = FILL_AREA_STYLE_COLOUR ( '', #6578 ) ;
#15464 = COLOUR_RGB ( '', 0.66274510, 0.83137255, 0.94901961) ;
#15465 = AXIS2_PLACEMENT_3D ( 'NONE', #1598, #7517, #20165 ) ;
#15466 = VECTOR ( 'NONE', #9041, 1000.000000000000000 ) ;
#15467 = EDGE_CURVE ( 'NONE', #14575, #1752, #13999, .T. ) ;
#15468 = ORIENTED_EDGE ( 'NONE', *, *, #12413, .F. ) ;
#15469 = ORIENTED_EDGE ( 'NONE', *, *, #10744, .F. ) ;
#15470 = EDGE_LOOP ( 'NONE', ( #1614, #12813 ) ) ;
#15471 = EDGE_CURVE ( 'NONE', #530, #738, #6362, .T. ) ;
#15472 = DIRECTION ( 'NONE',  ( 1.000000000000000000, -0.000000000000000000, -0.000000000000000000 ) ) ;
#15473 = ORIENTED_EDGE ( 'NONE', *, *, #18117, .F. ) ;
#15474 = ORIENTED_EDGE ( 'NONE', *, *, #16352, .F. ) ;
#15475 = VERTEX_POINT ( 'NONE', #12645 ) ;
#15476 = CARTESIAN_POINT ( 'NONE',  ( -40.00000000000000000, 19.00000000000000000, 25.99999999999999645 ) ) ;
#15477 = EDGE_CURVE ( 'NONE', #8912, #3482, #18618, .T. ) ;
#15478 = CARTESIAN_POINT ( 'NONE',  ( -79.99999999999995737, 316.7545334744432353, 515.1946179577817020 ) ) ;
#15479 = UNCERTAINTY_MEASURE_WITH_UNIT (LENGTH_MEASURE( 1.000000000000000082E-05 ), #11285, 'distance_accuracy_value', 'NONE');
#15480 = FACE_OUTER_BOUND ( 'NONE', #19599, .T. ) ;
#15481 =( NAMED_UNIT ( * ) PLANE_ANGLE_UNIT ( ) SI_UNIT ( $, .RADIAN. ) );
#15482 = STYLED_ITEM ( 'NONE', ( #1810 ), #16487 ) ;
#15483 = CARTESIAN_POINT ( 'NONE',  ( 498.8334540492693918, 191.8198460455371333, 24.99421986894476078 ) ) ;
#15484 = AXIS2_PLACEMENT_3D ( 'NONE', #12716, #10953, #18969 ) ;
#15485 = CARTESIAN_POINT ( 'NONE',  ( 0.000000000000000000, 0.000000000000000000, 35.00000000000000711 ) ) ;
#15486 = DIRECTION ( 'NONE',  ( 0.000000000000000000, -0.000000000000000000, 1.000000000000000000 ) ) ;
#15487 = CARTESIAN_POINT ( 'NONE',  ( 30.99999999999999645, 68.00000000000000000, 31.00000000000001066 ) ) ;
#15488 = CARTESIAN_POINT ( 'NONE',  ( 0.2538567052040897609, 139.5545947507227709, 500.3746700499490885 ) ) ;
#15489 = ORIENTED_EDGE ( 'NONE', *, *, #19068, .F. ) ;
#15490 = DIRECTION ( 'NONE',  ( 0.000000000000000000, 0.000000000000000000, 1.000000000000000000 ) ) ;
#15491 = LINE ( 'NONE', #18664, #18876 ) ;
#15492 = DIRECTION ( 'NONE',  ( -0.000000000000000000, -1.000000000000000000, 0.000000000000000000 ) ) ;
#15493 = AXIS2_PLACEMENT_3D ( 'NONE', #5829, #11909, #8715 ) ;
#15494 = CIRCLE ( 'NONE', #17118, 3.300000000000025135 ) ;
#15495 = AXIS2_PLACEMENT_3D ( 'NONE', #16037, #330, #13137 ) ;
#15496 = EDGE_CURVE ( 'NONE', #323, #9433, #4605, .T. ) ;
#15497 = PRESENTATION_LAYER_ASSIGNMENT (  '', '', ( #2296 ) ) ;
#15498 = VERTEX_POINT ( 'NONE', #1366 ) ;
#15499 = DIRECTION ( 'NONE',  ( 0.000000000000000000, -0.000000000000000000, -1.000000000000000000 ) ) ;
#15500 = EDGE_LOOP ( 'NONE', ( #6296, #18179 ) ) ;
#15501 = CARTESIAN_POINT ( 'NONE',  ( 26.00000000000000355, 19.00000000000000000, -31.00000000000004263 ) ) ;
#15502 = DIRECTION ( 'NONE',  ( 2.135044278125300850E-16, -1.000000000000000000, 0.000000000000000000 ) ) ;
#15503 = VERTEX_POINT ( 'NONE', #9338 ) ;
#15504 = LINE ( 'NONE', #15913, #19909 ) ;
#15505 = CARTESIAN_POINT ( 'NONE',  ( 406.3334540492693350, 167.8734308960555950, 0.000000000000000000 ) ) ;
#15506 = CARTESIAN_POINT ( 'NONE',  ( 463.8334540492693350, 191.8198460455371333, 168.2339398819845826 ) ) ;
#15507 = AXIS2_PLACEMENT_3D ( 'NONE', #2302, #3970, #8906 ) ;
#15508 = CARTESIAN_POINT ( 'NONE',  ( -31.81980515339462912, 0.000000000000000000, 35.11980515339465825 ) ) ;
#15509 = STYLED_ITEM ( 'NONE', ( #19101 ), #7251 ) ;
#15510 = CARTESIAN_POINT ( 'NONE',  ( 17.99999999999998224, 6.000000000000000000, -35.99999999999999289 ) ) ;
#15511 = DIRECTION ( 'NONE',  ( 0.000000000000000000, -1.000000000000000000, 0.000000000000000000 ) ) ;
#15512 = CARTESIAN_POINT ( 'NONE',  ( -211.5106270998635409, 103.1299228374912360, 79.58252780074349175 ) ) ;
#15513 = ORIENTED_EDGE ( 'NONE', *, *, #11309, .T. ) ;
#15514 = CARTESIAN_POINT ( 'NONE',  ( -1.135258727068400654E-15, 216.7545334744432921, 478.3411705753777596 ) ) ;
#15515 = VERTEX_POINT ( 'NONE', #4818 ) ;
#15516 = DIRECTION ( 'NONE',  ( 1.000000000000000000, 0.000000000000000000, -1.156482317317883755E-15 ) ) ;
#15517 = DIRECTION ( 'NONE',  ( 0.000000000000000000, 0.000000000000000000, 1.000000000000000000 ) ) ;
#15518 = PRODUCT ( '722909', '722909', '', ( #3017 ) ) ;
#15519 = EDGE_LOOP ( 'NONE', ( #5208, #5669, #17643, #1515 ) ) ;
#15520 = ORIENTED_EDGE ( 'NONE', *, *, #17057, .T. ) ;
#15521 = FACE_OUTER_BOUND ( 'NONE', #619, .T. ) ;
#15522 = ORIENTED_EDGE ( 'NONE', *, *, #561, .F. ) ;
#15523 = ORIENTED_EDGE ( 'NONE', *, *, #19595, .T. ) ;
#15524 = EDGE_CURVE ( 'NONE', #5614, #2877, #18915, .T. ) ;
#15525 = VERTEX_POINT ( 'NONE', #16987 ) ;
#15526 = AXIS2_PLACEMENT_3D ( 'NONE', #10303, #902, #2471 ) ;
#15527 = TOROIDAL_SURFACE ( 'NONE', #12896, 8.000000000000000000, 1.000000000000000000 ) ;
#15528 = LINE ( 'NONE', #18604, #1474 ) ;
#15529 = ORIENTED_EDGE ( 'NONE', *, *, #17144, .F. ) ;
#15530 = CARTESIAN_POINT ( 'NONE',  ( 0.2770853660078497760, 140.6978508428007615, 501.1291105955846206 ) ) ;
#15531 = ORIENTED_EDGE ( 'NONE', *, *, #585, .T. ) ;
#15532 = DIRECTION ( 'NONE',  ( 0.000000000000000000, 0.7071067811865445751, 0.7071067811865504593 ) ) ;
#15533 = DIRECTION ( 'NONE',  ( 0.000000000000000000, 1.000000000000000000, -1.224646799147353207E-16 ) ) ;
#15534 = APPLICATION_CONTEXT ( 'automotive_design' ) ;
#15535 = CARTESIAN_POINT ( 'NONE',  ( 98.48937290013662960, 103.1299228374914208, 29.36128450348865471 ) ) ;
#15536 = PRESENTATION_STYLE_ASSIGNMENT (( #10778 ) ) ;
#15537 = LINE ( 'NONE', #18704, #6037 ) ;
#15538 = CARTESIAN_POINT ( 'NONE',  ( 21.00000000000000000, 19.00000000000000000, 31.00000000000006395 ) ) ;
#15539 = DIRECTION ( 'NONE',  ( 1.000000000000000000, 0.000000000000000000, 1.156482317317870344E-15 ) ) ;
#15540 = ADVANCED_FACE ( 'NONE', ( #11093, #14280, #12441, #15852, #10686 ), #4701, .T. ) ;
#15541 = COLOUR_RGB ( '', 0.08235294, 0.09019608, 0.10196078) ;
#15542 = DIRECTION ( 'NONE',  ( 0.000000000000000000, 0.000000000000000000, 1.000000000000000000 ) ) ;
#15543 = DIRECTION ( 'NONE',  ( 0.000000000000000000, 0.000000000000000000, 1.000000000000000000 ) ) ;
#15544 = DIRECTION ( 'NONE',  ( 2.135044278125301096E-16, -1.000000000000000000, 0.000000000000000000 ) ) ;
#15545 = CARTESIAN_POINT ( 'NONE',  ( 0.000000000000000000, 0.000000000000000000, -135.0000000000000284 ) ) ;
#15546 = CARTESIAN_POINT ( 'NONE',  ( -79.99999999999995737, 146.8256012863087108, 507.0490161104376057 ) ) ;
#15547 = FILL_AREA_STYLE ('',( #17169 ) ) ;
#15548 = EDGE_LOOP ( 'NONE', ( #16017, #19271, #15903, #16773 ) ) ;
#15549 = VERTEX_POINT ( 'NONE', #9136 ) ;
#15550 = EDGE_CURVE ( 'NONE', #14419, #15780, #13141, .T. ) ;
#15551 = ORIENTED_EDGE ( 'NONE', *, *, #1919, .T. ) ;
#15552 = DIRECTION ( 'NONE',  ( -1.000000000000000000, -0.000000000000000000, -3.328238341717372086E-14 ) ) ;
#15553 = AXIS2_PLACEMENT_3D ( 'NONE', #6764, #13052, #19302 ) ;
#15554 = ORIENTED_EDGE ( 'NONE', *, *, #11001, .T. ) ;
#15555 = DIRECTION ( 'NONE',  ( 1.000000000000000000, 5.889072920838430686E-16, -0.000000000000000000 ) ) ;
#15556 = CARTESIAN_POINT ( 'NONE',  ( 463.8334540492693350, 191.8198460455371333, 215.0057801310552179 ) ) ;
#15557 = EDGE_CURVE ( 'NONE', #8401, #12469, #8570, .T. ) ;
#15558 = VECTOR ( 'NONE', #13274, 1000.000000000000000 ) ;
#15559 = EDGE_LOOP ( 'NONE', ( #14689, #1778, #11097, #20289 ) ) ;
#15560 =( NAMED_UNIT ( * ) PLANE_ANGLE_UNIT ( ) SI_UNIT ( $, .RADIAN. ) );
#15561 = DIRECTION ( 'NONE',  ( -0.000000000000000000, 0.000000000000000000, 1.000000000000000000 ) ) ;
#15562 = DIRECTION ( 'NONE',  ( 0.000000000000000000, 0.000000000000000000, 1.000000000000000000 ) ) ;
#15563 = SURFACE_STYLE_USAGE ( .BOTH. , #9253 ) ;
#15564 = DIRECTION ( 'NONE',  ( 0.000000000000000000, 1.000000000000000000, 0.000000000000000000 ) ) ;
#15565 = FILL_AREA_STYLE_COLOUR ( '', #17882 ) ;
#15566 = EDGE_CURVE ( 'NONE', #12714, #19684, #11190, .T. ) ;
#15567 = ORIENTED_EDGE ( 'NONE', *, *, #446, .F. ) ;
#15568 = CARTESIAN_POINT ( 'NONE',  ( -38.50085094405407204, 209.4098724938429541, 505.3921618609452935 ) ) ;
#15569 = EDGE_CURVE ( 'NONE', #18513, #3196, #5501, .T. ) ;
#15570 =( GEOMETRIC_REPRESENTATION_CONTEXT ( 3 ) GLOBAL_UNCERTAINTY_ASSIGNED_CONTEXT ( ( #16519 ) ) GLOBAL_UNIT_ASSIGNED_CONTEXT ( ( #13685, #15124, #3995 ) ) REPRESENTATION_CONTEXT ( 'NONE', 'WORKASPACE' ) );
#15571 = PRESENTATION_LAYER_ASSIGNMENT (  '', '', ( #15905 ) ) ;
#15572 = CIRCLE ( 'NONE', #13260, 8.000000000000000000 ) ;
#15573 = ORIENTED_EDGE ( 'NONE', *, *, #9768, .F. ) ;
#15574 = EDGE_LOOP ( 'NONE', ( #7875, #14300, #12319, #11916 ) ) ;
#15575 = ORIENTED_EDGE ( 'NONE', *, *, #14897, .F. ) ;
#15576 = DIRECTION ( 'NONE',  ( 0.000000000000000000, 1.000000000000000000, 0.000000000000000000 ) ) ;
#15577 = EDGE_CURVE ( 'NONE', #5039, #14898, #5399, .T. ) ;
#15578 = PRESENTATION_LAYER_ASSIGNMENT (  '', '', ( #9974 ) ) ;
#15579 = CARTESIAN_POINT ( 'NONE',  ( 10.00000000000000000, 309.2289037985885898, -79.88019484660914316 ) ) ;
#15580 = ORIENTED_EDGE ( 'NONE', *, *, #8211, .F. ) ;
#15581 = AXIS2_PLACEMENT_3D ( 'NONE', #11881, #2494, #18552 ) ;
#15582 = ORIENTED_EDGE ( 'NONE', *, *, #1901, .T. ) ;
#15583 = EDGE_LOOP ( 'NONE', ( #12543, #2313 ) ) ;
#15584 = CARTESIAN_POINT ( 'NONE',  ( 40.00000000000000000, 0.000000000000000000, 26.00000000000000355 ) ) ;
#15585 = DIRECTION ( 'NONE',  ( 0.000000000000000000, -1.000000000000000000, 0.000000000000000000 ) ) ;
#15586 = DIRECTION ( 'NONE',  ( 0.000000000000000000, 1.000000000000000000, 0.000000000000000000 ) ) ;
#15587 = VECTOR ( 'NONE', #3741, 1000.000000000000000 ) ;
#15588 = VECTOR ( 'NONE', #1364, 1000.000000000000000 ) ;
#15589 = LINE ( 'NONE', #17503, #10079 ) ;
#15590 = EDGE_CURVE ( 'NONE', #15549, #865, #15971, .T. ) ;
#15591 = ORIENTED_EDGE ( 'NONE', *, *, #16220, .T. ) ;
#15592 = DIRECTION ( 'NONE',  ( -0.000000000000000000, -1.000000000000000000, -0.000000000000000000 ) ) ;
#15593 = CARTESIAN_POINT ( 'NONE',  ( 133.4893729001365443, 123.1299228374914634, 170.4174721992565082 ) ) ;
#15594 = DIRECTION ( 'NONE',  ( 0.000000000000000000, 1.000000000000000000, 0.000000000000000000 ) ) ;
#15595 = EDGE_CURVE ( 'NONE', #8340, #368, #12315, .T. ) ;
#15596 = LINE ( 'NONE', #9579, #11604 ) ;
#15597 =( LENGTH_UNIT ( ) NAMED_UNIT ( * ) SI_UNIT ( .MILLI., .METRE. ) );
#15598 = ORIENTED_EDGE ( 'NONE', *, *, #19949, .T. ) ;
#15599 = PRESENTATION_LAYER_ASSIGNMENT (  '', '', ( #4391 ) ) ;
#15600 = CARTESIAN_POINT ( 'NONE',  ( 31.81980515339464333, 11.00000000000000000, 31.81980515339463622 ) ) ;
#15601 = PLANE ( 'NONE',  #16610 ) ;
#15602 = LINE ( 'NONE', #5071, #8384 ) ;
#15603 = AXIS2_PLACEMENT_3D ( 'NONE', #18753, #8049, #3204 ) ;
#15604 = ORIENTED_EDGE ( 'NONE', *, *, #12835, .T. ) ;
#15605 = AXIS2_PLACEMENT_3D ( 'NONE', #9625, #17454, #15947 ) ;
#15606 = PLANE ( 'NONE',  #17168 ) ;
#15607 = ORIENTED_EDGE ( 'NONE', *, *, #5623, .T. ) ;
#15608 = ADVANCED_FACE ( 'NONE', ( #9641 ), #17960, .F. ) ;
#15609 = SURFACE_STYLE_FILL_AREA ( #3002 ) ;
#15610 = LINE ( 'NONE', #4466, #8888 ) ;
#15611 = ORIENTED_EDGE ( 'NONE', *, *, #6146, .T. ) ;
#15612 = DIRECTION ( 'NONE',  ( -1.000000000000000000, 0.000000000000000000, -0.000000000000000000 ) ) ;
#15613 = CARTESIAN_POINT ( 'NONE',  ( -7.005190481990339112E-15, 37.39913938097243573, -5.741599279633704455E-16 ) ) ;
#15614 = EDGE_CURVE ( 'NONE', #5765, #17495, #16292, .T. ) ;
#15615 = MECHANICAL_DESIGN_GEOMETRIC_PRESENTATION_REPRESENTATION (  '', ( #9341 ), #17239 ) ;
#15616 = PRESENTATION_LAYER_ASSIGNMENT (  '', '', ( #1415 ) ) ;
#15617 = CARTESIAN_POINT ( 'NONE',  ( -0.06893388336922114112, 140.7261352223151505, 502.2905978699745333 ) ) ;
#15618 = LINE ( 'NONE', #4879, #14407 ) ;
#15619 = FACE_OUTER_BOUND ( 'NONE', #6737, .T. ) ;
#15620 = CIRCLE ( 'NONE', #8689, 2.500000000000002220 ) ;
#15621 = DIRECTION ( 'NONE',  ( 0.000000000000000000, 0.000000000000000000, 1.000000000000000000 ) ) ;
#15622 = VERTEX_POINT ( 'NONE', #13235 ) ;
#15623 = DIRECTION ( 'NONE',  ( 1.156482317317883755E-15, -0.000000000000000000, 1.000000000000000000 ) ) ;
#15624 = CARTESIAN_POINT ( 'NONE',  ( 0.000000000000000000, 0.000000000000000000, 245.0000000000000000 ) ) ;
#15625 = APPLICATION_PROTOCOL_DEFINITION ( 'draft international standard', 'automotive_design', 1998, #16850 ) ;
#15626 = AXIS2_PLACEMENT_3D ( 'NONE', #9501, #12409, #6433 ) ;
#15627 = ORIENTED_EDGE ( 'NONE', *, *, #4308, .F. ) ;
#15628 = ORIENTED_EDGE ( 'NONE', *, *, #18698, .T. ) ;
#15629 = AXIS2_PLACEMENT_3D ( 'NONE', #510, #13409, #11850 ) ;
#15630 = ORIENTED_EDGE ( 'NONE', *, *, #11903, .F. ) ;
#15631 = ORIENTED_EDGE ( 'NONE', *, *, #8450, .F. ) ;
#15632 = ORIENTED_EDGE ( 'NONE', *, *, #11818, .F. ) ;
#15633 = CIRCLE ( 'NONE', #14631, 10.00000000000000888 ) ;
#15634 = AXIS2_PLACEMENT_3D ( 'NONE', #10306, #11864, #10416 ) ;
#15635 = AXIS2_PLACEMENT_3D ( 'NONE', #19696, #7560, #13742 ) ;
#15636 = DIRECTION ( 'NONE',  ( 1.000000000000000000, 0.000000000000000000, 0.000000000000000000 ) ) ;
#15637 = VECTOR ( 'NONE', #215, 1000.000000000000000 ) ;
#15638 = ORIENTED_EDGE ( 'NONE', *, *, #16578, .T. ) ;
#15639 = CARTESIAN_POINT ( 'NONE',  ( 498.8334540492693918, 191.8198460455371333, 81.76606011801540319 ) ) ;
#15640 = CARTESIAN_POINT ( 'NONE',  ( 0.000000000000000000, 316.7545334744432353, 495.1946179577816451 ) ) ;
#15641 = VECTOR ( 'NONE', #12807, 1000.000000000000000 ) ;
#15642 = CARTESIAN_POINT ( 'NONE',  ( -31.00000000000001776, 0.000000000000000000, 31.00000000000000000 ) ) ;
#15643 = VECTOR ( 'NONE', #12552, 1000.000000000000000 ) ;
#15644 = SURFACE_SIDE_STYLE ('',( #9327 ) ) ;
#15645 = STYLED_ITEM ( 'NONE', ( #4874 ), #10404 ) ;
#15646 = DIRECTION ( 'NONE',  ( -1.000000000000000000, 0.000000000000000000, -0.000000000000000000 ) ) ;
#15647 = DIRECTION ( 'NONE',  ( -1.000000000000000000, -5.889072920838430686E-16, 0.000000000000000000 ) ) ;
#15648 = EDGE_CURVE ( 'NONE', #10793, #18104, #15620, .T. ) ;
#15649 = CARTESIAN_POINT ( 'NONE',  ( 31.00000000000000000, 19.00000000000000000, 30.99999999999999289 ) ) ;
#15650 = ORIENTED_EDGE ( 'NONE', *, *, #13024, .T. ) ;
#15651 = CARTESIAN_POINT ( 'NONE',  ( 498.8117674897343932, 191.8198460455371333, 225.0057801310552463 ) ) ;
#15652 = MECHANICAL_DESIGN_GEOMETRIC_PRESENTATION_REPRESENTATION (  '', ( #3794 ), #19547 ) ;
#15653 = CARTESIAN_POINT ( 'NONE',  ( 3.850000000000000089, -14.27500000000000036, -1.768083816268991068E-15 ) ) ;
#15655 = VECTOR ( 'NONE', #17800, 1000.000000000000000 ) ;
#15654 = SURFACE_SIDE_STYLE ('',( #15434 ) ) ;
#15656 = FACE_BOUND ( 'NONE', #3402, .T. ) ;
#15657 = DIRECTION ( 'NONE',  ( 0.000000000000000000, 1.224646799147356165E-16, 1.000000000000000000 ) ) ;
#15658 = VERTEX_POINT ( 'NONE', #8115 ) ;
#15659 = VECTOR ( 'NONE', #11556, 1000.000000000000000 ) ;
#15660 = ORIENTED_EDGE ( 'NONE', *, *, #10339, .T. ) ;
#15661 = COLOUR_RGB ( '', 0.40784314, 0.44705882, 0.49803922) ;
#15662 = ORIENTED_EDGE ( 'NONE', *, *, #12663, .F. ) ;
#15663 = VERTEX_POINT ( 'NONE', #10330 ) ;
#15664 = DIRECTION ( 'NONE',  ( 0.000000000000000000, 0.000000000000000000, 1.000000000000000000 ) ) ;
#15665 = EDGE_CURVE ( 'NONE', #7572, #3235, #2271, .T. ) ;
#15666 = CARTESIAN_POINT ( 'NONE',  ( 78.48937290013660117, 145.9162550801369491, -140.0000000000001137 ) ) ;
#15667 = ORIENTED_EDGE ( 'NONE', *, *, #12411, .T. ) ;
#15668 = SURFACE_SIDE_STYLE ('',( #18927 ) ) ;
#15669 = VECTOR ( 'NONE', #1140, 1000.000000000000000 ) ;
#15670 = CARTESIAN_POINT ( 'NONE',  ( 498.8334540492693918, 191.8198460455371333, 91.76606011801541740 ) ) ;
#15671 = ORIENTED_EDGE ( 'NONE', *, *, #17986, .F. ) ;
#15672 = PLANE ( 'NONE',  #3947 ) ;
#15673 = CARTESIAN_POINT ( 'NONE',  ( 0.000000000000000000, 10.00000000000000000, 0.000000000000000000 ) ) ;
#15674 = VECTOR ( 'NONE', #20002, 1000.000000000000000 ) ;
#15675 = CARTESIAN_POINT ( 'NONE',  ( -39.99999999999999289, 11.00000000000000000, 25.99999999999999645 ) ) ;
#15676 = ORIENTED_EDGE ( 'NONE', *, *, #1411, .T. ) ;
#15677 = CARTESIAN_POINT ( 'NONE',  ( -2.903217335657449993, 60.78097370076725525, 9.045605051663343943 ) ) ;
#15678 = AXIS2_PLACEMENT_3D ( 'NONE', #5000, #3150, #8095 ) ;
#15679 =( LENGTH_UNIT ( ) NAMED_UNIT ( * ) SI_UNIT ( .MILLI., .METRE. ) );
#15680 = LINE ( 'NONE', #7722, #9543 ) ;
#15681 = CARTESIAN_POINT ( 'NONE',  ( 468.8334540492694487, 134.2156642432025251, 245.0000000000000000 ) ) ;
#15682 = EDGE_CURVE ( 'NONE', #995, #19309, #19004, .T. ) ;
#15683 = ORIENTED_EDGE ( 'NONE', *, *, #9804, .F. ) ;
#15684 = CARTESIAN_POINT ( 'NONE',  ( -30.99999999999999289, 0.000000000000000000, 31.00000000000000000 ) ) ;
#15685 = CARTESIAN_POINT ( 'NONE',  ( 463.8334540492693350, 191.8198460455371333, 215.0057801310552179 ) ) ;
#15686 = EDGE_CURVE ( 'NONE', #9496, #18212, #11574, .T. ) ;
#15687 = ORIENTED_EDGE ( 'NONE', *, *, #18666, .F. ) ;
#15688 = EDGE_LOOP ( 'NONE', ( #16549, #3782, #10905, #357 ) ) ;
#15689 = VERTEX_POINT ( 'NONE', #8483 ) ;
#15690 = VECTOR ( 'NONE', #16823, 1000.000000000000000 ) ;
#15691 = SURFACE_SIDE_STYLE ('',( #10929 ) ) ;
#15692 = VERTEX_POINT ( 'NONE', #14763 ) ;
#15693 = ORIENTED_EDGE ( 'NONE', *, *, #12010, .F. ) ;
#15694 = ORIENTED_EDGE ( 'NONE', *, *, #876, .T. ) ;
#15695 = SURFACE_SIDE_STYLE ('',( #13613 ) ) ;
#15696 = AXIS2_PLACEMENT_3D ( 'NONE', #7534, #7834, #8963 ) ;
#15697 = CARTESIAN_POINT ( 'NONE',  ( -211.5106270998635409, 113.1299228374912502, 220.6387154965113382 ) ) ;
#15698 = DIRECTION ( 'NONE',  ( 1.000000000000000000, 0.000000000000000000, 0.000000000000000000 ) ) ;
#15699 = EDGE_CURVE ( 'NONE', #18646, #7052, #10439, .T. ) ;
#15700 = CARTESIAN_POINT ( 'NONE',  ( -118.0000000000000284, 216.7545334744432921, 205.1946179577815883 ) ) ;
#15701 = CARTESIAN_POINT ( 'NONE',  ( -75.00000000000000000, 313.8311070602663904, -87.78239810828596035 ) ) ;
#15702 = LINE ( 'NONE', #16826, #412 ) ;
#15703 = LINE ( 'NONE', #1739, #7066 ) ;
#15704 = SURFACE_SIDE_STYLE ('',( #1311 ) ) ;
#15705 = AXIS2_PLACEMENT_3D ( 'NONE', #13595, #1188, #4525 ) ;
#15706 = CARTESIAN_POINT ( 'NONE',  ( -0.3492608071101708234, 139.7605458594808567, 500.8004217433215217 ) ) ;
#15707 = EDGE_CURVE ( 'NONE', #11471, #11867, #10739, .T. ) ;
#15708 = ORIENTED_EDGE ( 'NONE', *, *, #3355, .F. ) ;
#15709 =( NAMED_UNIT ( * ) PLANE_ANGLE_UNIT ( ) SI_UNIT ( $, .RADIAN. ) );
#15710 = EDGE_CURVE ( 'NONE', #14418, #18003, #10013, .T. ) ;
#15711 = EDGE_CURVE ( 'NONE', #17040, #5279, #18453, .T. ) ;
#15712 = ORIENTED_EDGE ( 'NONE', *, *, #1852, .T. ) ;
#15713 = EDGE_CURVE ( 'NONE', #6449, #7874, #15491, .T. ) ;
#15714 =( LENGTH_UNIT ( ) NAMED_UNIT ( * ) SI_UNIT ( .MILLI., .METRE. ) );
#15715 = ORIENTED_EDGE ( 'NONE', *, *, #18151, .F. ) ;
#15716 = EDGE_CURVE ( 'NONE', #5827, #6868, #5075, .T. ) ;
#15717 = DIRECTION ( 'NONE',  ( -0.000000000000000000, -1.000000000000000000, -0.000000000000000000 ) ) ;
#15718 = CARTESIAN_POINT ( 'NONE',  ( 78.48937290013662960, 1.675782865040797740E-14, 0.000000000000000000 ) ) ;
#15719 = EDGE_LOOP ( 'NONE', ( #5763, #15861, #11080, #19424 ) ) ;
#15720 = DIRECTION ( 'NONE',  ( 0.000000000000000000, 0.000000000000000000, -1.000000000000000000 ) ) ;
#15721 = DIRECTION ( 'NONE',  ( 0.000000000000000000, 0.000000000000000000, 1.000000000000000000 ) ) ;
#15722 = DIRECTION ( 'NONE',  ( 0.000000000000000000, 0.000000000000000000, -1.000000000000000000 ) ) ;
#15723 = CARTESIAN_POINT ( 'NONE',  ( 35.00000000000000711, 0.000000000000000000, 35.00000000000000711 ) ) ;
#15724 = CARTESIAN_POINT ( 'NONE',  ( 10.00000000000000000, 306.0487089519832011, -75.00000000000380851 ) ) ;
#15725 =( NAMED_UNIT ( * ) SI_UNIT ( $, .STERADIAN. ) SOLID_ANGLE_UNIT ( ) );
#15726 = ORIENTED_EDGE ( 'NONE', *, *, #12395, .T. ) ;
#15727 = CARTESIAN_POINT ( 'NONE',  ( 78.48937290013660117, 123.1299228374914208, 79.58252780074349175 ) ) ;
#15728 = DIRECTION ( 'NONE',  ( 0.000000000000000000, 0.000000000000000000, -1.000000000000000000 ) ) ;
#15729 = DIRECTION ( 'NONE',  ( -1.000000000000000000, 0.000000000000000000, 0.000000000000000000 ) ) ;
#15730 = APPLICATION_PROTOCOL_DEFINITION ( 'draft international standard', 'automotive_design', 1998, #366 ) ;
#15731 = SURFACE_SIDE_STYLE ('',( #12736 ) ) ;
#15732 = VERTEX_POINT ( 'NONE', #4167 ) ;
#15733 = ORIENTED_EDGE ( 'NONE', *, *, #20174, .F. ) ;
#15734 = EDGE_LOOP ( 'NONE', ( #8152, #6888, #7528, #16301 ) ) ;
#15735 = ADVANCED_FACE ( 'NONE', ( #13626 ), #15601, .T. ) ;
#15736 = CARTESIAN_POINT ( 'NONE',  ( 31.00000000000003553, 19.00000000000000000, 25.99999999999999645 ) ) ;
#15737 = ADVANCED_FACE ( 'NONE', ( #10838 ), #16931, .F. ) ;
#15738 = ORIENTED_EDGE ( 'NONE', *, *, #17051, .F. ) ;
#15739 = MANIFOLD_SOLID_BREP ( 'Boss-Extrude3', #13926 ) ;
#15740 = AXIS2_PLACEMENT_3D ( 'NONE', #18874, #9413, #12503 ) ;
#15741 = ADVANCED_FACE ( 'NONE', ( #3419 ), #8884, .T. ) ;
#15742 = EDGE_LOOP ( 'NONE', ( #5757, #5950, #17841, #14556 ) ) ;
#15743 = CARTESIAN_POINT ( 'NONE',  ( 19.99999999999995381, 0.000000000000000000, -39.99999999999999289 ) ) ;
#15744 = CARTESIAN_POINT ( 'NONE',  ( 4.549999999999999822, 1.748183305782846567E-15, 14.27500000000000036 ) ) ;
#15745 = CIRCLE ( 'NONE', #1209, 2.500000000000002220 ) ;
#15746 = CARTESIAN_POINT ( 'NONE',  ( -81.18192946989263703, 147.7545334744432921, 496.6642397995874489 ) ) ;
#15747 = DIRECTION ( 'NONE',  ( 0.000000000000000000, 0.000000000000000000, -1.000000000000000000 ) ) ;
#15748 = FILL_AREA_STYLE ('',( #1890 ) ) ;
#15749 = DIRECTION ( 'NONE',  ( -0.000000000000000000, 1.000000000000000000, -0.000000000000000000 ) ) ;
#15750 = VERTEX_POINT ( 'NONE', #7947 ) ;
#15751 = SURFACE_STYLE_FILL_AREA ( #14079 ) ;
#15752 = PLANE ( 'NONE',  #10283 ) ;
#15753 = DIRECTION ( 'NONE',  ( 1.000000000000000000, 0.000000000000000000, 0.000000000000000000 ) ) ;
#15754 = CARTESIAN_POINT ( 'NONE',  ( -31.00000000000002842, 0.000000000000000000, 31.00000000000000000 ) ) ;
#15755 = CARTESIAN_POINT ( 'NONE',  ( 30.99999999999995737, 3.000000000000000000, 31.00000000000000000 ) ) ;
#15756 = DIRECTION ( 'NONE',  ( 0.000000000000000000, 1.000000000000000000, 0.000000000000000000 ) ) ;
#15757 = VERTEX_POINT ( 'NONE', #12589 ) ;
#15758 = AXIS2_PLACEMENT_3D ( 'NONE', #10475, #2637, #2938 ) ;
#15759 = EDGE_CURVE ( 'NONE', #11717, #2815, #17636, .T. ) ;
#15760 = ORIENTED_EDGE ( 'NONE', *, *, #9046, .T. ) ;
#15761 = CARTESIAN_POINT ( 'NONE',  ( 463.8334540492693350, 214.2156642432025251, -87.31255586191144857 ) ) ;
#15762 = CARTESIAN_POINT ( 'NONE',  ( -80.07925520782436024, 141.0520093089742204, 501.4288824830859426 ) ) ;
#15763 = ORIENTED_EDGE ( 'NONE', *, *, #15048, .T. ) ;
#15764 = CARTESIAN_POINT ( 'NONE',  ( 153.4893729001366864, 103.1299228374914492, 79.58252780074349175 ) ) ;
#15765 = DIRECTION ( 'NONE',  ( 0.000000000000000000, 0.000000000000000000, -1.000000000000000000 ) ) ;
#15766 = ORIENTED_EDGE ( 'NONE', *, *, #16058, .F. ) ;
#15767 = FACE_BOUND ( 'NONE', #9276, .T. ) ;
#15768 = LINE ( 'NONE', #7915, #16863 ) ;
#15769 = FILL_AREA_STYLE ('',( #12668 ) ) ;
#15770 = AXIS2_PLACEMENT_3D ( 'NONE', #1040, #15194, #7565 ) ;
#15771 = CARTESIAN_POINT ( 'NONE',  ( -38.50085094405407204, 193.0431417881923153, 505.3921618609452935 ) ) ;
#15772 = LINE ( 'NONE', #6693, #3565 ) ;
#15773 = LINE ( 'NONE', #10917, #3061 ) ;
#15774 = CARTESIAN_POINT ( 'NONE',  ( -38.50085094405407204, 159.0821755739672483, 505.3921618609452935 ) ) ;
#15775 = DIRECTION ( 'NONE',  ( 1.000000000000000000, 6.763469278324249959E-16, 4.651923389110021175E-16 ) ) ;
#15776 = FACE_OUTER_BOUND ( 'NONE', #16008, .T. ) ;
#15777 = ORIENTED_EDGE ( 'NONE', *, *, #19712, .T. ) ;
#15778 = ORIENTED_EDGE ( 'NONE', *, *, #13636, .F. ) ;
#15779 = UNCERTAINTY_MEASURE_WITH_UNIT (LENGTH_MEASURE( 1.000000000000000082E-05 ), #7156, 'distance_accuracy_value', 'NONE');
#15780 = VERTEX_POINT ( 'NONE', #12 ) ;
#15781 = ORIENTED_EDGE ( 'NONE', *, *, #7791, .T. ) ;
#15782 = ORIENTED_EDGE ( 'NONE', *, *, #10292, .F. ) ;
#15783 = DIRECTION ( 'NONE',  ( 0.000000000000000000, 0.000000000000000000, -1.000000000000000000 ) ) ;
#15784 = DIRECTION ( 'NONE',  ( 1.000000000000000000, 5.889072920838430686E-16, -0.000000000000000000 ) ) ;
#15785 = LINE ( 'NONE', #15888, #5643 ) ;
#15786 = FACE_OUTER_BOUND ( 'NONE', #14039, .T. ) ;
#15787 = ORIENTED_EDGE ( 'NONE', *, *, #288, .T. ) ;
#15788 = DIRECTION ( 'NONE',  ( -0.000000000000000000, 1.000000000000000000, 0.000000000000000000 ) ) ;
#15789 = PRODUCT_DEFINITION ( 'UNKNOWN', '', #17516, #5550 ) ;
#15790 = VECTOR ( 'NONE', #9466, 1000.000000000000000 ) ;
#15791 = FACE_OUTER_BOUND ( 'NONE', #8613, .T. ) ;
#15792 = CARTESIAN_POINT ( 'NONE',  ( -21.85283368562565443, 319.7545334744432353, 485.1700099148404774 ) ) ;
#15793 = AXIS2_PLACEMENT_3D ( 'NONE', #3502, #6697, #6813 ) ;
#15794 = ORIENTED_EDGE ( 'NONE', *, *, #819, .T. ) ;
#15795 = VECTOR ( 'NONE', #963, 1000.000000000000000 ) ;
#15796 = DIRECTION ( 'NONE',  ( -1.000000000000000000, -0.000000000000000000, -0.000000000000000000 ) ) ;
#15797 = EDGE_CURVE ( 'NONE', #6152, #11717, #18222, .T. ) ;
#15798 = DIRECTION ( 'NONE',  ( -1.000000000000000000, 0.000000000000000000, 0.000000000000000000 ) ) ;
#15799 = ORIENTED_EDGE ( 'NONE', *, *, #10125, .F. ) ;
#15800 =( REPRESENTATION_RELATIONSHIP ('NONE','NONE', #13279, #8923 ) REPRESENTATION_RELATIONSHIP_WITH_TRANSFORMATION ( #8288 )SHAPE_REPRESENTATION_RELATIONSHIP( ) );
#15801 = EDGE_CURVE ( 'NONE', #39, #20118, #15900, .T. ) ;
#15802 = AXIS2_PLACEMENT_3D ( 'NONE', #6663, #8202, #14474 ) ;
#15803 = DIRECTION ( 'NONE',  ( -1.000000000000000000, 0.000000000000000000, 0.000000000000000000 ) ) ;
#15804 = ORIENTED_EDGE ( 'NONE', *, *, #8227, .T. ) ;
#15805 = DIRECTION ( 'NONE',  ( 0.000000000000000000, 0.000000000000000000, -1.000000000000000000 ) ) ;
#15806 = ORIENTED_EDGE ( 'NONE', *, *, #19952, .T. ) ;
#15807 = CARTESIAN_POINT ( 'NONE',  ( 0.000000000000000000, 3.000000000000000888, -150.0000000000000000 ) ) ;
#15808 =( NAMED_UNIT ( * ) PLANE_ANGLE_UNIT ( ) SI_UNIT ( $, .RADIAN. ) );
#15809 = EDGE_CURVE ( 'NONE', #4266, #1021, #11235, .T. ) ;
#15810 = CARTESIAN_POINT ( 'NONE',  ( -0.01348608808930003983, 140.1729642737128927, 501.5297937275371964 ) ) ;
#15811 = EDGE_CURVE ( 'NONE', #20015, #645, #11344, .T. ) ;
#15812 = CYLINDRICAL_SURFACE ( 'NONE', #15740, 3.000000000000002665 ) ;
#15813 = DIRECTION ( 'NONE',  ( 0.000000000000000000, 0.000000000000000000, -1.000000000000000000 ) ) ;
#15814 = CARTESIAN_POINT ( 'NONE',  ( 108.9893729001366154, 131.2883416677199193, 282.8521325859589979 ) ) ;
#15815 = EDGE_LOOP ( 'NONE', ( #10205, #10659, #7256, #15155 ) ) ;
#15816 = LINE ( 'NONE', #3442, #14438 ) ;
#15817 = CARTESIAN_POINT ( 'NONE',  ( 0.000000000000000000, 0.000000000000000000, 250.0000000000000000 ) ) ;
#15818 = EDGE_CURVE ( 'NONE', #8090, #5003, #12490, .T. ) ;
#15819 = DIRECTION ( 'NONE',  ( 0.000000000000000000, 0.000000000000000000, -1.000000000000000000 ) ) ;
#15820 = AXIS2_PLACEMENT_3D ( 'NONE', #18373, #5521, #4274 ) ;
#15821 = ITEM_DEFINED_TRANSFORMATION ( 'NONE', 'NONE', #7692,  #2741 ) ;
#15822 = EDGE_CURVE ( 'NONE', #18716, #5319, #7085, .T. ) ;
#15823 = AXIS2_PLACEMENT_3D ( 'NONE', #1354, #10878, #7884 ) ;
#15824 = CIRCLE ( 'NONE', #16162, 10.00000000000000888 ) ;
#15825 = ORIENTED_EDGE ( 'NONE', *, *, #1677, .F. ) ;
#15826 = EDGE_LOOP ( 'NONE', ( #5021, #16135, #5138, #19249, #2251, #9101, #7932, #17861 ) ) ;
#15827 = DIRECTION ( 'NONE',  ( 1.000000000000000000, 1.197852309262419498E-15, -0.000000000000000000 ) ) ;
#15828 = EDGE_CURVE ( 'NONE', #11725, #6461, #14436, .T. ) ;
#15829 = VERTEX_POINT ( 'NONE', #9805 ) ;
#15830 = ORIENTED_EDGE ( 'NONE', *, *, #5012, .F. ) ;
#15831 = ORIENTED_EDGE ( 'NONE', *, *, #2189, .F. ) ;
#15832 = CARTESIAN_POINT ( 'NONE',  ( 53.48937290013659407, 129.7247684487574588, 368.0000000000000000 ) ) ;
#15833 = EDGE_CURVE ( 'NONE', #8577, #8093, #16021, .T. ) ;
#15834 = VERTEX_POINT ( 'NONE', #9400 ) ;
#15835 = LINE ( 'NONE', #3029, #11322 ) ;
#15836 = CIRCLE ( 'NONE', #6953, 8.000000000000000000 ) ;
#15837 = FILL_AREA_STYLE ('',( #9622 ) ) ;
#15838 = ORIENTED_EDGE ( 'NONE', *, *, #3952, .T. ) ;
#15839 = STYLED_ITEM ( 'NONE', ( #9814 ), #7362 ) ;
#15840 = DIRECTION ( 'NONE',  ( -0.000000000000000000, -0.000000000000000000, 1.000000000000000000 ) ) ;
#15841 = AXIS2_PLACEMENT_3D ( 'NONE', #6640, #19387, #11571 ) ;
#15842 = DIRECTION ( 'NONE',  ( -0.8502651466878615727, -0.5263546146162958461, -6.445984940062853155E-17 ) ) ;
#15843 = SURFACE_SIDE_STYLE ('',( #18904 ) ) ;
#15844 = CARTESIAN_POINT ( 'NONE',  ( 31.81980515339464333, 8.000000000000000000, -35.11980515339463693 ) ) ;
#15845 = DIRECTION ( 'NONE',  ( 0.000000000000000000, 0.000000000000000000, -1.000000000000000000 ) ) ;
#15846 = COLOUR_RGB ( '', 0.08235294, 0.09019608, 0.10196078) ;
#15847 = ORIENTED_EDGE ( 'NONE', *, *, #20138, .F. ) ;
#15848 = LINE ( 'NONE', #6671, #4881 ) ;
#15849 = CARTESIAN_POINT ( 'NONE',  ( 21.99999999999998224, 8.000000000000000000, -32.99999999999999289 ) ) ;
#15850 = DIRECTION ( 'NONE',  ( 0.000000000000000000, 0.000000000000000000, 1.000000000000000000 ) ) ;
#15851 = CARTESIAN_POINT ( 'NONE',  ( 25.99999999999998224, 10.00000000000000000, -31.99999999999998579 ) ) ;
#15852 = FACE_BOUND ( 'NONE', #15470, .T. ) ;
#15853 = CARTESIAN_POINT ( 'NONE',  ( 178.4893729001365728, 113.1299228374914918, 79.58252780074349175 ) ) ;
#15854 = CARTESIAN_POINT ( 'NONE',  ( -0.06173851122038213207, 138.7995772466921949, 490.1653550096017966 ) ) ;
#15855 = DIRECTION ( 'NONE',  ( 1.000000000000000000, -0.000000000000000000, -0.000000000000000000 ) ) ;
#15856 = VECTOR ( 'NONE', #3503, 1000.000000000000000 ) ;
#15857 = VECTOR ( 'NONE', #16820, 1000.000000000000000 ) ;
#15858 = VERTEX_POINT ( 'NONE', #8163 ) ;
#15859 =( LENGTH_UNIT ( ) NAMED_UNIT ( * ) SI_UNIT ( .MILLI., .METRE. ) );
#15860 = CARTESIAN_POINT ( 'NONE',  ( -79.99999999999995737, 140.8764026050587290, 502.4686618848273270 ) ) ;
#15861 = ORIENTED_EDGE ( 'NONE', *, *, #9162, .T. ) ;
#15862 = FACE_OUTER_BOUND ( 'NONE', #9813, .T. ) ;
#15863 = DIRECTION ( 'NONE',  ( 0.000000000000000000, 1.000000000000000000, 0.000000000000000000 ) ) ;
#15864 = EDGE_CURVE ( 'NONE', #6099, #18945, #8056, .T. ) ;
#15865 = EDGE_LOOP ( 'NONE', ( #7931, #1203, #8783, #3151, #8265 ) ) ;
#15866 = LINE ( 'NONE', #12666, #18750 ) ;
#15867 = CIRCLE ( 'NONE', #13871, 1.000000000000000888 ) ;
#15868 = CARTESIAN_POINT ( 'NONE',  ( -33.99999999999997158, 3.000000000000000000, -25.99999999999999645 ) ) ;
#15869 = CARTESIAN_POINT ( 'NONE',  ( 153.4893729001366580, 0.000000000000000000, -97.94896630388704750 ) ) ;
#15870 = DIRECTION ( 'NONE',  ( -0.000000000000000000, -0.000000000000000000, 1.000000000000000000 ) ) ;
#15871 = COLOUR_RGB ( '', 0.40784314, 0.44705882, 0.49803922) ;
#15872 = DIRECTION ( 'NONE',  ( 1.000000000000000000, -0.000000000000000000, 0.000000000000000000 ) ) ;
#15873 = MANIFOLD_SOLID_BREP ( 'Cut-Extrude4[2]', #13605 ) ;
#15874 = DIRECTION ( 'NONE',  ( -1.000000000000000000, 0.000000000000000000, 0.000000000000000000 ) ) ;
#15875 = DIRECTION ( 'NONE',  ( -0.000000000000000000, 1.000000000000000000, 7.137148015447440312E-15 ) ) ;
#15876 = CARTESIAN_POINT ( 'NONE',  ( -26.00000000000002842, 0.000000000000000000, 34.00000000000000711 ) ) ;
#15877 = FACE_OUTER_BOUND ( 'NONE', #15583, .T. ) ;
#15878 = DIRECTION ( 'NONE',  ( 0.000000000000000000, 0.000000000000000000, -1.000000000000000000 ) ) ;
#15879 = EDGE_LOOP ( 'NONE', ( #11319, #6915, #11884, #14341 ) ) ;
#15880 =( GEOMETRIC_REPRESENTATION_CONTEXT ( 3 ) GLOBAL_UNCERTAINTY_ASSIGNED_CONTEXT ( ( #5985 ) ) GLOBAL_UNIT_ASSIGNED_CONTEXT ( ( #8719, #13466, #5621 ) ) REPRESENTATION_CONTEXT ( 'NONE', 'WORKASPACE' ) );
#15881 = ORIENTED_EDGE ( 'NONE', *, *, #8750, .T. ) ;
#15882 = FILL_AREA_STYLE ('',( #15369 ) ) ;
#15883 = VERTEX_POINT ( 'NONE', #7845 ) ;
#15884 = EDGE_LOOP ( 'NONE', ( #19008, #7831, #14582, #13380 ) ) ;
#15885 = ORIENTED_EDGE ( 'NONE', *, *, #12184, .T. ) ;
#15886 = CARTESIAN_POINT ( 'NONE',  ( 53.48937290013659407, 127.7247684487574304, 250.0000000000000000 ) ) ;
#15887 =( LENGTH_UNIT ( ) NAMED_UNIT ( * ) SI_UNIT ( .MILLI., .METRE. ) );
#15888 = CARTESIAN_POINT ( 'NONE',  ( 149.0892156028631348, 167.9162550801369491, 245.0000000000000000 ) ) ;
#15889 = AXIS2_PLACEMENT_3D ( 'NONE', #13278, #5444, #9225 ) ;
#15890 = FACE_OUTER_BOUND ( 'NONE', #17445, .T. ) ;
#15891 = CARTESIAN_POINT ( 'NONE',  ( -40.00000000000000000, 19.00000000000000000, 25.99999999999999645 ) ) ;
#15892 = CARTESIAN_POINT ( 'NONE',  ( 25.99999999999998224, 6.000000000000000000, -31.99999999999998579 ) ) ;
#15893 =( NAMED_UNIT ( * ) SI_UNIT ( $, .STERADIAN. ) SOLID_ANGLE_UNIT ( ) );
#15894 = STYLED_ITEM ( 'NONE', ( #18401 ), #13523 ) ;
#15895 = PLANE ( 'NONE',  #14571 ) ;
#15896 = CARTESIAN_POINT ( 'NONE',  ( 178.4893729001366012, 34.32473510485366575, -140.0000000000001137 ) ) ;
#15897 = EDGE_CURVE ( 'NONE', #1482, #1591, #3109, .T. ) ;
#15898 = STYLED_ITEM ( 'NONE', ( #7684 ), #8261 ) ;
#15899 = VERTEX_POINT ( 'NONE', #409 ) ;
#15900 = LINE ( 'NONE', #14343, #1437 ) ;
#15901 = LINE ( 'NONE', #6422, #8722 ) ;
#15902 = AXIS2_PLACEMENT_3D ( 'NONE', #15746, #15951, #1573 ) ;
#15903 = ORIENTED_EDGE ( 'NONE', *, *, #10485, .F. ) ;
#15904 = CIRCLE ( 'NONE', #15234, 15.25000000000000000 ) ;
#15905 = STYLED_ITEM ( 'NONE', ( #10785 ), #18171 ) ;
#15906 = EDGE_CURVE ( 'NONE', #19309, #10163, #9703, .T. ) ;
#15907 = CYLINDRICAL_SURFACE ( 'NONE', #12191, 10.00000000000000888 ) ;
#15908 = EDGE_LOOP ( 'NONE', ( #15660, #14215, #12053, #17624 ) ) ;
#15909 = EDGE_CURVE ( 'NONE', #13635, #15261, #6424, .T. ) ;
#15910 =( NAMED_UNIT ( * ) PLANE_ANGLE_UNIT ( ) SI_UNIT ( $, .RADIAN. ) );
#15911 =( NAMED_UNIT ( * ) SI_UNIT ( $, .STERADIAN. ) SOLID_ANGLE_UNIT ( ) );
#15912 = ORIENTED_EDGE ( 'NONE', *, *, #18288, .F. ) ;
#15913 = CARTESIAN_POINT ( 'NONE',  ( 153.4893729001366580, 80.91625508013694912, -97.94896630388704750 ) ) ;
#15914 = DIRECTION ( 'NONE',  ( -0.000000000000000000, -1.000000000000000000, -0.000000000000000000 ) ) ;
#15915 = CARTESIAN_POINT ( 'NONE',  ( 503.8334540492693918, 191.8198460455371333, 34.99421986894476788 ) ) ;
#15916 = VECTOR ( 'NONE', #8462, 1000.000000000000000 ) ;
#15917 = CARTESIAN_POINT ( 'NONE',  ( 0.7125494648445551693, 139.4936479042385997, 500.2362377901696959 ) ) ;
#15918 = LINE ( 'NONE', #28, #11788 ) ;
#15919 = CARTESIAN_POINT ( 'NONE',  ( 1.181929469892510243, 139.7703989349544145, 490.5655098179848892 ) ) ;
#15920 = DIRECTION ( 'NONE',  ( 0.000000000000000000, 1.000000000000000000, 0.000000000000000000 ) ) ;
#15921 = PLANE ( 'NONE',  #8720 ) ;
#15922 = ORIENTED_EDGE ( 'NONE', *, *, #978, .T. ) ;
#15923 = CARTESIAN_POINT ( 'NONE',  ( -40.00000000000000000, 0.000000000000000000, 26.00000000000000355 ) ) ;
#15924 = LINE ( 'NONE', #6646, #6299 ) ;
#15925 = AXIS2_PLACEMENT_3D ( 'NONE', #20196, #6306, #18960 ) ;
#15926 = VECTOR ( 'NONE', #4394, 1000.000000000000000 ) ;
#15927 = APPLICATION_PROTOCOL_DEFINITION ( 'draft international standard', 'automotive_design', 1998, #15534 ) ;
#15928 = EDGE_CURVE ( 'NONE', #13587, #2876, #3780, .T. ) ;
#15929 = ORIENTED_EDGE ( 'NONE', *, *, #18797, .F. ) ;
#15930 = ORIENTED_EDGE ( 'NONE', *, *, #10136, .F. ) ;
#15931 = DIRECTION ( 'NONE',  ( 0.000000000000000000, 0.000000000000000000, -1.000000000000000000 ) ) ;
#15932 = ORIENTED_EDGE ( 'NONE', *, *, #13919, .F. ) ;
#15933 = VERTEX_POINT ( 'NONE', #14533 ) ;
#15934 = ADVANCED_FACE ( 'NONE', ( #13316 ), #18896, .F. ) ;
#15935 = CONICAL_SURFACE ( 'NONE', #4720, 14.43750000000000000, 0.7483780475235185525 ) ;
#15936 = ORIENTED_EDGE ( 'NONE', *, *, #6008, .T. ) ;
#15937 = DIRECTION ( 'NONE',  ( 1.000000000000000000, 0.000000000000000000, 0.000000000000000000 ) ) ;
#15938 = DIRECTION ( 'NONE',  ( 0.000000000000000000, -2.775557561562888827E-14, -1.000000000000000000 ) ) ;
#15939 = VERTEX_POINT ( 'NONE', #14955 ) ;
#15940 = AXIS2_PLACEMENT_3D ( 'NONE', #11111, #1710, #12559 ) ;
#15941 = SURFACE_STYLE_USAGE ( .BOTH. , #12743 ) ;
#15942 = MECHANICAL_DESIGN_GEOMETRIC_PRESENTATION_REPRESENTATION (  '', ( #8025 ), #13612 ) ;
#15943 = CARTESIAN_POINT ( 'NONE',  ( 10.00000000000000000, 372.8685141053783241, -146.8198051533979935 ) ) ;
#15944 = ORIENTED_EDGE ( 'NONE', *, *, #5767, .T. ) ;
#15945 = ADVANCED_FACE ( 'NONE', ( #3828 ), #19658, .F. ) ;
#15946 = MECHANICAL_DESIGN_GEOMETRIC_PRESENTATION_REPRESENTATION (  '', ( #13948 ), #8999 ) ;
#15947 = DIRECTION ( 'NONE',  ( 0.000000000000000000, 0.000000000000000000, -1.000000000000000000 ) ) ;
#15948 = DIRECTION ( 'NONE',  ( 0.000000000000000000, -0.000000000000000000, 1.000000000000000000 ) ) ;
#15949 = EDGE_CURVE ( 'NONE', #7872, #8092, #145, .T. ) ;
#15950 = DIRECTION ( 'NONE',  ( 0.000000000000000000, 1.000000000000000000, 0.000000000000000000 ) ) ;
#15951 = DIRECTION ( 'NONE',  ( 1.000000000000000000, 0.000000000000000000, 3.328238341717372086E-14 ) ) ;
#15952 =( NAMED_UNIT ( * ) SI_UNIT ( $, .STERADIAN. ) SOLID_ANGLE_UNIT ( ) );
#15953 = AXIS2_PLACEMENT_3D ( 'NONE', #18972, #15914, #14663 ) ;
#15954 = CARTESIAN_POINT ( 'NONE',  ( -2.600106608147766174, 39.49089379158813529, 9.137947797636652325 ) ) ;
#15955 = ORIENTED_EDGE ( 'NONE', *, *, #5922, .T. ) ;
#15956 = DIRECTION ( 'NONE',  ( -9.815121534730718631E-17, 1.000000000000000000, 0.000000000000000000 ) ) ;
#15957 = DIRECTION ( 'NONE',  ( -9.815121534730717399E-17, 1.000000000000000000, 0.000000000000000000 ) ) ;
#15958 = DIRECTION ( 'NONE',  ( 1.000000000000000000, 0.000000000000000000, 0.000000000000000000 ) ) ;
#15959 = DIRECTION ( 'NONE',  ( 2.597405907254919044E-19, 0.7791332379872890623, 0.6268583551835632539 ) ) ;
#15960 =( NAMED_UNIT ( * ) PLANE_ANGLE_UNIT ( ) SI_UNIT ( $, .RADIAN. ) );
#15961 = CARTESIAN_POINT ( 'NONE',  ( 0.000000000000000000, 5.000000000000000888, -150.0000000000000000 ) ) ;
#15962 = STYLED_ITEM ( 'NONE', ( #10141 ), #10198 ) ;
#15963 = CARTESIAN_POINT ( 'NONE',  ( 0.000000000000000000, 381.0487089519837127, -150.0000000000032685 ) ) ;
#15964 = EDGE_CURVE ( 'NONE', #14816, #8147, #12669, .T. ) ;
#15965 = CARTESIAN_POINT ( 'NONE',  ( -0.8244006410038320354, 138.9529133135991401, 489.1850737022905378 ) ) ;
#15966 =( LENGTH_UNIT ( ) NAMED_UNIT ( * ) SI_UNIT ( .MILLI., .METRE. ) );
#15967 = MECHANICAL_DESIGN_GEOMETRIC_PRESENTATION_REPRESENTATION (  '', ( #8383 ), #782 ) ;
#15968 = ORIENTED_EDGE ( 'NONE', *, *, #14201, .T. ) ;
#15969 = MECHANICAL_DESIGN_GEOMETRIC_PRESENTATION_REPRESENTATION (  '', ( #18871 ), #11312 ) ;
#15970 = AXIS2_PLACEMENT_3D ( 'NONE', #1940, #9110, #7172 ) ;
#15971 = CIRCLE ( 'NONE', #2420, 5.000000000000000888 ) ;
#15972 = EDGE_LOOP ( 'NONE', ( #11504, #15929, #10309, #13690 ) ) ;
#15973 = CARTESIAN_POINT ( 'NONE',  ( -20.99999999999999645, 19.00000000000000000, 35.00000000000001421 ) ) ;
#15974 = EDGE_CURVE ( 'NONE', #6215, #1279, #1947, .T. ) ;
#15975 = STYLED_ITEM ( 'NONE', ( #8035 ), #1709 ) ;
#15976 = VECTOR ( 'NONE', #19015, 1000.000000000000000 ) ;
#15977 = ORIENTED_EDGE ( 'NONE', *, *, #9932, .F. ) ;
#15978 =( NAMED_UNIT ( * ) PLANE_ANGLE_UNIT ( ) SI_UNIT ( $, .RADIAN. ) );
#15979 = CARTESIAN_POINT ( 'NONE',  ( -80.51897068092245036, 140.5128581817066902, 500.9441570819607250 ) ) ;
#15980 = VECTOR ( 'NONE', #18571, 1000.000000000000000 ) ;
#15981 = ORIENTED_EDGE ( 'NONE', *, *, #15220, .T. ) ;
#15982 = EDGE_CURVE ( 'NONE', #8633, #3886, #16948, .T. ) ;
#15983 = PLANE ( 'NONE',  #20211 ) ;
#15984 = CARTESIAN_POINT ( 'NONE',  ( -31.00000000000003553, 19.00000000000000000, 25.99999999999999645 ) ) ;
#15985 = VERTEX_POINT ( 'NONE', #2041 ) ;
#15986 = AXIS2_PLACEMENT_3D ( 'NONE', #16235, #7965, #16039 ) ;
#15987 = CARTESIAN_POINT ( 'NONE',  ( 178.4893729001365728, 103.1299228374914776, 79.58252780074349175 ) ) ;
#15988 = CARTESIAN_POINT ( 'NONE',  ( 31.00000000000001421, 10.00000000000000000, 22.99999999999999645 ) ) ;
#15989 = FACE_BOUND ( 'NONE', #447, .T. ) ;
#15990 = DIRECTION ( 'NONE',  ( 0.000000000000000000, 1.000000000000000000, 0.000000000000000000 ) ) ;
#15991 = DIRECTION ( 'NONE',  ( 0.000000000000000000, 0.000000000000000000, 1.000000000000000000 ) ) ;
#15992 = FACE_OUTER_BOUND ( 'NONE', #2875, .T. ) ;
#15993 = CARTESIAN_POINT ( 'NONE',  ( -31.81980515339462912, 11.00000000000000000, -35.11980515339465114 ) ) ;
#15994 = VECTOR ( 'NONE', #1814, 1000.000000000000000 ) ;
#15995 = CARTESIAN_POINT ( 'NONE',  ( -22.00000000000001776, 8.000000000000000000, 36.00000000000000711 ) ) ;
#15996 = ORIENTED_EDGE ( 'NONE', *, *, #13828, .F. ) ;
#15997 = CIRCLE ( 'NONE', #7088, 10.00000000000000888 ) ;
#15998 = LINE ( 'NONE', #20282, #4656 ) ;
#15999 = LINE ( 'NONE', #195, #15131 ) ;
#16000 = ORIENTED_EDGE ( 'NONE', *, *, #9385, .T. ) ;
#16001 = VECTOR ( 'NONE', #1508, 1000.000000000000000 ) ;
#16002 = EDGE_CURVE ( 'NONE', #18143, #18212, #4018, .T. ) ;
#16003 = ORIENTED_EDGE ( 'NONE', *, *, #19145, .F. ) ;
#16004 = AXIS2_PLACEMENT_3D ( 'NONE', #13623, #5395, #2380 ) ;
#16005 = ORIENTED_EDGE ( 'NONE', *, *, #11269, .F. ) ;
#16006 = UNCERTAINTY_MEASURE_WITH_UNIT (LENGTH_MEASURE( 1.000000000000000082E-05 ), #18745, 'distance_accuracy_value', 'NONE');
#16007 = ORIENTED_EDGE ( 'NONE', *, *, #1293, .T. ) ;
#16008 = EDGE_LOOP ( 'NONE', ( #19028, #3394, #6337, #20268 ) ) ;
#16009 = EDGE_CURVE ( 'NONE', #11820, #19489, #4434, .T. ) ;
#16010 = VERTEX_POINT ( 'NONE', #8658 ) ;
#16011 = CARTESIAN_POINT ( 'NONE',  ( 463.8334540492693350, 191.8198460455371333, 81.76606011801540319 ) ) ;
#16012 = AXIS2_PLACEMENT_3D ( 'NONE', #11463, #8278, #3639 ) ;
#16013 = FACE_OUTER_BOUND ( 'NONE', #1384, .T. ) ;
#16014 = ADVANCED_FACE ( 'NONE', ( #19566 ), #610, .T. ) ;
#16015 = STYLED_ITEM ( 'NONE', ( #10870 ), #9032 ) ;
#16016 = CARTESIAN_POINT ( 'NONE',  ( -31.00000000000007105, 10.00000000000000000, 23.00000000000000000 ) ) ;
#16017 = ORIENTED_EDGE ( 'NONE', *, *, #14033, .T. ) ;
#16018 = SURFACE_STYLE_FILL_AREA ( #6829 ) ;
#16019 =( NAMED_UNIT ( * ) SI_UNIT ( $, .STERADIAN. ) SOLID_ANGLE_UNIT ( ) );
#16020 = SURFACE_SIDE_STYLE ('',( #5472 ) ) ;
#16021 = LINE ( 'NONE', #12705, #13970 ) ;
#16022 = CARTESIAN_POINT ( 'NONE',  ( 0.000000000000000000, -3.000000000000000000, 0.000000000000000000 ) ) ;
#16023 = STYLED_ITEM ( 'NONE', ( #4445 ), #2545 ) ;
#16024 = VERTEX_POINT ( 'NONE', #13713 ) ;
#16025 = VERTEX_POINT ( 'NONE', #10415 ) ;
#16026 = EDGE_CURVE ( 'NONE', #4192, #10668, #18577, .T. ) ;
#16027 = DIRECTION ( 'NONE',  ( 0.000000000000000000, 1.000000000000000000, 0.000000000000000000 ) ) ;
#16028 = VERTEX_POINT ( 'NONE', #7316 ) ;
#16029 = CARTESIAN_POINT ( 'NONE',  ( -22.00000000000001776, 6.000000000000000000, 32.00000000000000711 ) ) ;
#16030 = ORIENTED_EDGE ( 'NONE', *, *, #10828, .T. ) ;
#16031 = LINE ( 'NONE', #18868, #1472 ) ;
#16032 = CIRCLE ( 'NONE', #1166, 4.999999999999997335 ) ;
#16033 = LINE ( 'NONE', #2264, #12268 ) ;
#16034 =( GEOMETRIC_REPRESENTATION_CONTEXT ( 3 ) GLOBAL_UNCERTAINTY_ASSIGNED_CONTEXT ( ( #11705 ) ) GLOBAL_UNIT_ASSIGNED_CONTEXT ( ( #2654, #7512, #13780 ) ) REPRESENTATION_CONTEXT ( 'NONE', 'WORKASPACE' ) );
#16035 = DIRECTION ( 'NONE',  ( 0.000000000000000000, 1.000000000000000000, -0.000000000000000000 ) ) ;
#16036 = DIRECTION ( 'NONE',  ( -1.135258727068398879E-15, 3.469446951953611033E-15, 1.000000000000000000 ) ) ;
#16037 = CARTESIAN_POINT ( 'NONE',  ( 1.181929469892510243, 138.7545334744432637, 490.5655098179833544 ) ) ;
#16038 = FACE_OUTER_BOUND ( 'NONE', #8560, .T. ) ;
#16039 = DIRECTION ( 'NONE',  ( 0.000000000000000000, 1.000000000000000000, 0.000000000000000000 ) ) ;
#16040 = ORIENTED_EDGE ( 'NONE', *, *, #2884, .F. ) ;
#16041 = CARTESIAN_POINT ( 'NONE',  ( -78.99999999999995737, 140.1563709946295262, 488.5655098179835818 ) ) ;
#16042 = CARTESIAN_POINT ( 'NONE',  ( 31.00000000000001421, 0.000000000000000000, 22.99999999999999645 ) ) ;
#16043 =( NAMED_UNIT ( * ) PLANE_ANGLE_UNIT ( ) SI_UNIT ( $, .RADIAN. ) );
#16044 = PRODUCT_DEFINITION_SHAPE ( 'NONE', 'NONE',  #20381 ) ;
#16045 = VERTEX_POINT ( 'NONE', #10305 ) ;
#16046 = CARTESIAN_POINT ( 'NONE',  ( 31.00000000000004263, 0.000000000000000000, -25.99999999999999645 ) ) ;
#16047 = ORIENTED_EDGE ( 'NONE', *, *, #8578, .F. ) ;
#16048 = EDGE_CURVE ( 'NONE', #13854, #7676, #3458, .T. ) ;
#16049 = VERTEX_POINT ( 'NONE', #2669 ) ;
#16050 = ORIENTED_EDGE ( 'NONE', *, *, #8727, .F. ) ;
#16051 = ORIENTED_EDGE ( 'NONE', *, *, #10398, .F. ) ;
#16052 = AXIS2_PLACEMENT_3D ( 'NONE', #16679, #14599, #480 ) ;
#16053 = FILL_AREA_STYLE ('',( #11268 ) ) ;
#16054 = ORIENTED_EDGE ( 'NONE', *, *, #14307, .T. ) ;
#16055 = FILL_AREA_STYLE_COLOUR ( '', #19526 ) ;
#16056 = DIRECTION ( 'NONE',  ( 1.000000000000000000, -0.000000000000000000, -0.000000000000000000 ) ) ;
#16057 = ORIENTED_EDGE ( 'NONE', *, *, #9483, .T. ) ;
#16058 = EDGE_CURVE ( 'NONE', #11746, #11967, #5754, .T. ) ;
#16059 = LINE ( 'NONE', #14691, #16892 ) ;
#16060 = CARTESIAN_POINT ( 'NONE',  ( -31.00000000000005684, 68.00000000000000000, 23.00000000000000355 ) ) ;
#16061 = CARTESIAN_POINT ( 'NONE',  ( 1.347066989204613998E-15, 0.000000000000000000, 22.00000000000000000 ) ) ;
#16062 = VERTEX_POINT ( 'NONE', #18333 ) ;
#16063 = CARTESIAN_POINT ( 'NONE',  ( 55.98937290013660828, 130.3113892758443058, 284.0770112900635240 ) ) ;
#16064 =( NAMED_UNIT ( * ) SI_UNIT ( $, .STERADIAN. ) SOLID_ANGLE_UNIT ( ) );
#16065 = LINE ( 'NONE', #10061, #3033 ) ;
#16066 = CARTESIAN_POINT ( 'NONE',  ( 25.99999999999999645, 68.00000000000000000, 40.00000000000002132 ) ) ;
#16067 =( BOUNDED_SURFACE ( )  B_SPLINE_SURFACE ( 3, 2, ( 
 ( #14140, #14246, #230 ),
 ( #12603, #6225, #1550 ),
 ( #7774, #7861, #15917 ),
 ( #26, #3010, #14054 ),
 ( #4783, #123, #18873 ),
 ( #9505, #1456, #1761 ),
 ( #11065, #17343, #8076 ),
 ( #4983, #3226, #11253 ),
 ( #6436, #18773, #9304 ),
 ( #12502, #17535, #14452 ),
 ( #4569, #15810, #1648 ),
 ( #4878, #10851, #7962 ),
 ( #3437, #12723, #6133 ),
 ( #6531, #18975, #11154 ),
 ( #17432, #15617, #3324 ),
 ( #12819, #19075, #1864 ) ),
 .UNSPECIFIED., .F., .F., .T. ) 
 B_SPLINE_SURFACE_WITH_KNOTS ( ( 4, 2, 2, 2, 2, 2, 2, 4 ),
 ( 3, 3 ),
 ( 0.001246970379171045062, 0.001676325320858793304, 0.002105680262546541764, 0.002535035204234289789, 0.002964390145922038249, 0.003393745087609786708, 0.003823100029297534733, 0.004681809912673031218 ),
 ( 0.000000000000000000, 1.000000000000000000 ),
 .UNSPECIFIED. ) 
 GEOMETRIC_REPRESENTATION_ITEM ( )  RATIONAL_B_SPLINE_SURFACE ( (
 ( 1.000000000000000000, 0.8351454326190185240, 1.000000000000000000),
 ( 1.000000000000000000, 0.8351391024961110077, 1.000000000000000000),
 ( 1.000000000000000000, 0.8348195684913958248, 1.000000000000000000),
 ( 1.000000000000000000, 0.8333905549599697204, 1.000000000000000000),
 ( 1.000000000000000000, 0.8322627347962558986, 1.000000000000000000),
 ( 1.000000000000000000, 0.8289108061541168304, 1.000000000000000000),
 ( 1.000000000000000000, 0.8266665721634388619, 1.000000000000000000),
 ( 1.000000000000000000, 0.8205566980956985335, 1.000000000000000000),
 ( 1.000000000000000000, 0.8167651399558516490, 1.000000000000000000),
 ( 1.000000000000000000, 0.8072326331355020868, 1.000000000000000000),
 ( 1.000000000000000000, 0.8014496535022105350, 1.000000000000000000),
 ( 1.000000000000000000, 0.7879847800020959303, 1.000000000000000000),
 ( 1.000000000000000000, 0.7802402271099223574, 1.000000000000000000),
 ( 1.000000000000000000, 0.7537145741180295566, 1.000000000000000000),
 ( 1.000000000000000000, 0.7323456299789787849, 1.000000000000000000),
 ( 1.000000000000000000, 0.7071067811865475727, 1.000000000000000000) ) ) 
 REPRESENTATION_ITEM ( '' )  SURFACE ( )  );
#16068 = ORIENTED_EDGE ( 'NONE', *, *, #6463, .T. ) ;
#16069 = DIRECTION ( 'NONE',  ( -4.956352788505164254E-16, 0.000000000000000000, -1.000000000000000000 ) ) ;
#16070 = SURFACE_STYLE_USAGE ( .BOTH. , #14591 ) ;
#16071 = EDGE_CURVE ( 'NONE', #11592, #10771, #8951, .T. ) ;
#16072 = EDGE_LOOP ( 'NONE', ( #4516, #9928, #16396, #14710 ) ) ;
#16073 = ORIENTED_EDGE ( 'NONE', *, *, #4510, .T. ) ;
#16074 = EDGE_CURVE ( 'NONE', #6242, #5571, #17012, .T. ) ;
#16075 = VECTOR ( 'NONE', #16713, 1000.000000000000000 ) ;
#16076 = ORIENTED_EDGE ( 'NONE', *, *, #7475, .F. ) ;
#16077 = CARTESIAN_POINT ( 'NONE',  ( 498.8117674897343932, 214.2156642432025251, 0.000000000000000000 ) ) ;
#16078 = DIRECTION ( 'NONE',  ( 0.000000000000000000, -0.000000000000000000, -1.000000000000000000 ) ) ;
#16079 = ORIENTED_EDGE ( 'NONE', *, *, #14220, .F. ) ;
#16080 = ADVANCED_FACE ( 'NONE', ( #19869 ), #2870, .T. ) ;
#16081 = CARTESIAN_POINT ( 'NONE',  ( 30.99999999999997513, 10.00000000000000000, 25.99999999999999645 ) ) ;
#16082 = ADVANCED_FACE ( 'NONE', ( #7224 ), #10716, .F. ) ;
#16083 = CARTESIAN_POINT ( 'NONE',  ( -23.00000000000000000, 68.00000000000000000, -31.00000000000005684 ) ) ;
#16084 = VERTEX_POINT ( 'NONE', #3189 ) ;
#16085 = PLANE ( 'NONE',  #4941 ) ;
#16086 = CARTESIAN_POINT ( 'NONE',  ( 475.8334540492694487, 134.2156642432025251, 250.0000000000000000 ) ) ;
#16087 = EDGE_CURVE ( 'NONE', #865, #13434, #7827, .T. ) ;
#16088 = DIRECTION ( 'NONE',  ( 0.000000000000000000, 0.000000000000000000, -1.000000000000000000 ) ) ;
#16089 =( NAMED_UNIT ( * ) PLANE_ANGLE_UNIT ( ) SI_UNIT ( $, .RADIAN. ) );
#16090 = EDGE_CURVE ( 'NONE', #16423, #12769, #4938, .T. ) ;
#16091 = CARTESIAN_POINT ( 'NONE',  ( 30.99999999999997513, 0.000000000000000000, 25.99999999999999645 ) ) ;
#16092 = LINE ( 'NONE', #14412, #7877 ) ;
#16093 = ORIENTED_EDGE ( 'NONE', *, *, #12681, .F. ) ;
#16094 = FILL_AREA_STYLE ('',( #11839 ) ) ;
#16095 = FILL_AREA_STYLE_COLOUR ( '', #19105 ) ;
#16096 = ORIENTED_EDGE ( 'NONE', *, *, #4771, .F. ) ;
#16097 = ADVANCED_FACE ( 'NONE', ( #8143 ), #14014, .F. ) ;
#16098 = EDGE_CURVE ( 'NONE', #3235, #3148, #3393, .T. ) ;
#16099 = EDGE_LOOP ( 'NONE', ( #16670, #14210, #13465, #15009 ) ) ;
#16100 = ORIENTED_EDGE ( 'NONE', *, *, #18731, .T. ) ;
#16101 = DIRECTION ( 'NONE',  ( 0.000000000000000000, 0.000000000000000000, 1.000000000000000000 ) ) ;
#16102 = ORIENTED_EDGE ( 'NONE', *, *, #19885, .F. ) ;
#16103 = EDGE_LOOP ( 'NONE', ( #17639, #15081, #18436, #19467, #3667, #9493, #13126, #925 ) ) ;
#16104 = CYLINDRICAL_SURFACE ( 'NONE', #13704, 35.00000000000000711 ) ;
#16105 = ADVANCED_FACE ( 'NONE', ( #15776 ), #14415, .F. ) ;
#16106 = SURFACE_STYLE_FILL_AREA ( #8459 ) ;
#16107 = SURFACE_STYLE_USAGE ( .BOTH. , #9891 ) ;
#16108 = LINE ( 'NONE', #3, #15011 ) ;
#16109 = DIRECTION ( 'NONE',  ( -0.000000000000000000, -0.000000000000000000, 1.000000000000000000 ) ) ;
#16110 = CARTESIAN_POINT ( 'NONE',  ( 2.901926423773059760, 60.78602980190899530, 9.046021540735432964 ) ) ;
#16111 = DIRECTION ( 'NONE',  ( 0.000000000000000000, 0.000000000000000000, -1.000000000000000000 ) ) ;
#16112 = FACE_OUTER_BOUND ( 'NONE', #11006, .T. ) ;
#16113 = DIRECTION ( 'NONE',  ( 1.000000000000000000, 9.815121534730718631E-17, -0.000000000000000000 ) ) ;
#16114 = DIRECTION ( 'NONE',  ( 0.000000000000000000, 1.000000000000000000, 0.000000000000000000 ) ) ;
#16115 = EDGE_CURVE ( 'NONE', #12099, #1949, #286, .T. ) ;
#16116 = DIRECTION ( 'NONE',  ( -0.000000000000000000, 1.000000000000000000, -0.000000000000000000 ) ) ;
#16118 = EDGE_CURVE ( 'NONE', #10041, #9968, #15999, .T. ) ;
#16117 = AXIS2_PLACEMENT_3D ( 'NONE', #731, #10222, #11472 ) ;
#16119 = EDGE_CURVE ( 'NONE', #11823, #11321, #8220, .T. ) ;
#16120 = EDGE_LOOP ( 'NONE', ( #16516, #16486, #436, #4313 ) ) ;
#16121 = DIRECTION ( 'NONE',  ( 0.000000000000000000, -1.000000000000000000, 0.000000000000000000 ) ) ;
#16122 = UNCERTAINTY_MEASURE_WITH_UNIT (LENGTH_MEASURE( 1.000000000000000082E-05 ), #5616, 'distance_accuracy_value', 'NONE');
#16123 = VERTEX_POINT ( 'NONE', #15568 ) ;
#16124 = ORIENTED_EDGE ( 'NONE', *, *, #11980, .T. ) ;
#16125 = DIRECTION ( 'NONE',  ( 1.000000000000000000, -0.000000000000000000, -0.000000000000000000 ) ) ;
#16126 = UNCERTAINTY_MEASURE_WITH_UNIT (LENGTH_MEASURE( 1.000000000000000082E-05 ), #20166, 'distance_accuracy_value', 'NONE');
#16127 = ORIENTED_EDGE ( 'NONE', *, *, #3023, .F. ) ;
#16128 = FACE_BOUND ( 'NONE', #2977, .T. ) ;
#16129 = LINE ( 'NONE', #14550, #15587 ) ;
#16130 = AXIS2_PLACEMENT_3D ( 'NONE', #13103, #9284, #19026 ) ;
#16131 = DIRECTION ( 'NONE',  ( -9.815121534730717399E-17, 1.000000000000000000, 0.000000000000000000 ) ) ;
#16132 = CARTESIAN_POINT ( 'NONE',  ( 26.00000000000000711, 68.00000000000000000, -31.00000000000002487 ) ) ;
#16133 = CARTESIAN_POINT ( 'NONE',  ( 2.999999999999996891, 60.00000000000000711, 6.000000000000000000 ) ) ;
#16134 = PLANE ( 'NONE',  #4429 ) ;
#16135 = ORIENTED_EDGE ( 'NONE', *, *, #3957, .T. ) ;
#16136 = DIRECTION ( 'NONE',  ( 0.000000000000000000, 0.000000000000000000, -1.000000000000000000 ) ) ;
#16137 = CARTESIAN_POINT ( 'NONE',  ( 5.941205806953520074, 0.000000000000000000, 0.000000000000000000 ) ) ;
#16138 = DIRECTION ( 'NONE',  ( 1.000000000000000000, 0.000000000000000000, 0.000000000000000000 ) ) ;
#16139 = ITEM_DEFINED_TRANSFORMATION ( 'NONE', 'NONE', #20179,  #2741 ) ;
#16140 = EDGE_CURVE ( 'NONE', #3208, #19115, #18829, .T. ) ;
#16141 = CARTESIAN_POINT ( 'NONE',  ( 10.00000000000000000, 306.0487089519837696, -155.0000000000038369 ) ) ;
#16142 = ORIENTED_EDGE ( 'NONE', *, *, #8578, .T. ) ;
#16143 = AXIS2_PLACEMENT_3D ( 'NONE', #6489, #11119, #11024 ) ;
#16144 = VECTOR ( 'NONE', #19751, 1000.000000000000000 ) ;
#16145 =( GEOMETRIC_REPRESENTATION_CONTEXT ( 3 ) GLOBAL_UNCERTAINTY_ASSIGNED_CONTEXT ( ( #8526 ) ) GLOBAL_UNIT_ASSIGNED_CONTEXT ( ( #1369, #10479, #2746 ) ) REPRESENTATION_CONTEXT ( 'NONE', 'WORKASPACE' ) );
#16146 = ORIENTED_EDGE ( 'NONE', *, *, #4486, .F. ) ;
#16147 = ORIENTED_EDGE ( 'NONE', *, *, #15496, .F. ) ;
#16148 = DIRECTION ( 'NONE',  ( 0.6294249519366466039, 0.7770612780724246438, 0.000000000000000000 ) ) ;
#16149 = FACE_OUTER_BOUND ( 'NONE', #13244, .T. ) ;
#16150 = ORIENTED_EDGE ( 'NONE', *, *, #18011, .T. ) ;
#16151 = UNCERTAINTY_MEASURE_WITH_UNIT (LENGTH_MEASURE( 1.000000000000000082E-05 ), #8626, 'distance_accuracy_value', 'NONE');
#16152 = DIRECTION ( 'NONE',  ( -2.135044278125300850E-16, 1.000000000000000000, 0.000000000000000000 ) ) ;
#16153 = CARTESIAN_POINT ( 'NONE',  ( 2.181929469892510465, 216.7545334744432921, 490.5655098179832976 ) ) ;
#16154 = ORIENTED_EDGE ( 'NONE', *, *, #11816, .T. ) ;
#16155 = CARTESIAN_POINT ( 'NONE',  ( -20.00000000000003197, 3.000000000000000000, 40.00000000000000711 ) ) ;
#16156 = CARTESIAN_POINT ( 'NONE',  ( 88.88953019741013861, 167.9162550801369491, 245.0000000000000000 ) ) ;
#16157 = VECTOR ( 'NONE', #1072, 1000.000000000000000 ) ;
#16158 = DIRECTION ( 'NONE',  ( 0.000000000000000000, 0.000000000000000000, -1.000000000000000000 ) ) ;
#16159 = DIRECTION ( 'NONE',  ( 0.000000000000000000, 0.000000000000000000, -1.000000000000000000 ) ) ;
#16160 = CIRCLE ( 'NONE', #15146, 3.000000000000002665 ) ;
#16161 =( NAMED_UNIT ( * ) PLANE_ANGLE_UNIT ( ) SI_UNIT ( $, .RADIAN. ) );
#16162 = AXIS2_PLACEMENT_3D ( 'NONE', #11060, #17126, #10747 ) ;
#16163 = DIRECTION ( 'NONE',  ( -6.123031769111888756E-17, 1.000000000000000000, 3.749151804555344967E-33 ) ) ;
#16164 = ORIENTED_EDGE ( 'NONE', *, *, #8657, .F. ) ;
#16165 = DIRECTION ( 'NONE',  ( -0.000000000000000000, -0.000000000000000000, 1.000000000000000000 ) ) ;
#16166 = CARTESIAN_POINT ( 'NONE',  ( 10.00000000000000000, 372.8685141053778693, -83.18019484660869978 ) ) ;
#16167 = LINE ( 'NONE', #9754, #2716 ) ;
#16168 =( LENGTH_UNIT ( ) NAMED_UNIT ( * ) SI_UNIT ( .MILLI., .METRE. ) );
#16169 =( LENGTH_UNIT ( ) NAMED_UNIT ( * ) SI_UNIT ( .MILLI., .METRE. ) );
#16170 = EDGE_CURVE ( 'NONE', #2696, #15549, #4633, .T. ) ;
#16171 = LINE ( 'NONE', #9956, #15202 ) ;
#16172 = ORIENTED_EDGE ( 'NONE', *, *, #13213, .F. ) ;
#16173 = STYLED_ITEM ( 'NONE', ( #8857 ), #16557 ) ;
#16174 = AXIS2_PLACEMENT_3D ( 'NONE', #1671, #16793, #6453 ) ;
#16175 = PRESENTATION_LAYER_ASSIGNMENT (  '', '', ( #4631 ) ) ;
#16176 = VERTEX_POINT ( 'NONE', #15685 ) ;
#16177 = CARTESIAN_POINT ( 'NONE',  ( -80.20845338047620032, 140.7853878564479828, 501.2089312876914846 ) ) ;
#16178 = ORIENTED_EDGE ( 'NONE', *, *, #6356, .T. ) ;
#16179 = DIRECTION ( 'NONE',  ( -1.000000000000000000, 0.000000000000000000, 7.715811803773179210E-14 ) ) ;
#16180 = AXIS2_PLACEMENT_3D ( 'NONE', #7750, #20302, #12485 ) ;
#16181 = VERTEX_POINT ( 'NONE', #6392 ) ;
#16182 = EDGE_CURVE ( 'NONE', #12453, #17965, #3932, .T. ) ;
#16183 = DIRECTION ( 'NONE',  ( -0.000000000000000000, 1.000000000000000000, -0.000000000000000000 ) ) ;
#16184 = DIRECTION ( 'NONE',  ( 0.000000000000000000, 0.000000000000000000, 1.000000000000000000 ) ) ;
#16185 = DIRECTION ( 'NONE',  ( -0.000000000000000000, -1.000000000000000000, -0.000000000000000000 ) ) ;
#16186 = CARTESIAN_POINT ( 'NONE',  ( -35.00000000000000000, 8.000000000000000000, 20.99999999999999289 ) ) ;
#16187 = MECHANICAL_DESIGN_GEOMETRIC_PRESENTATION_REPRESENTATION (  '', ( #11208 ), #4643 ) ;
#16188 = FILL_AREA_STYLE ('',( #11314 ) ) ;
#16189 = DIRECTION ( 'NONE',  ( 0.000000000000000000, 0.000000000000000000, -1.000000000000000000 ) ) ;
#16190 = DIRECTION ( 'NONE',  ( 1.000000000000000000, 0.000000000000000000, 0.000000000000000000 ) ) ;
#16191 = DIRECTION ( 'NONE',  ( 1.000000000000000000, 5.889072920838430686E-16, -0.000000000000000000 ) ) ;
#16192 = ORIENTED_EDGE ( 'NONE', *, *, #11269, .T. ) ;
#16193 = ADVANCED_FACE ( 'NONE', ( #1719 ), #8030, .F. ) ;
#16194 = ORIENTED_EDGE ( 'NONE', *, *, #13547, .F. ) ;
#16195 = VERTEX_POINT ( 'NONE', #3808 ) ;
#16196 = EDGE_CURVE ( 'NONE', #2417, #3307, #790, .T. ) ;
#16197 = VERTEX_POINT ( 'NONE', #5250 ) ;
#16198 = VERTEX_POINT ( 'NONE', #8629 ) ;
#16199 = CARTESIAN_POINT ( 'NONE',  ( -81.18192946989111647, 138.7545334744432637, 489.5655098179833544 ) ) ;
#16200 = VECTOR ( 'NONE', #5454, 1000.000000000000000 ) ;
#16201 = FILL_AREA_STYLE ('',( #802 ) ) ;
#16202 = CARTESIAN_POINT ( 'NONE',  ( 17.99999999999998224, 10.00000000000000000, -35.99999999999999289 ) ) ;
#16203 = DIRECTION ( 'NONE',  ( -0.000000000000000000, -1.000000000000000000, -0.000000000000000000 ) ) ;
#16204 = EDGE_CURVE ( 'NONE', #10437, #13831, #16295, .T. ) ;
#16205 = DIRECTION ( 'NONE',  ( -0.000000000000000000, -1.000000000000000000, -0.000000000000000000 ) ) ;
#16206 = PRODUCT ( 'Part11^Assem2', 'Part11^Assem2', '', ( #16853 ) ) ;
#16207 = LINE ( 'NONE', #16311, #4055 ) ;
#16208 = FACE_OUTER_BOUND ( 'NONE', #7343, .T. ) ;
#16209 = SURFACE_SIDE_STYLE ('',( #16018 ) ) ;
#16210 = EDGE_CURVE ( 'NONE', #7788, #3926, #14512, .T. ) ;
#16211 = FACE_OUTER_BOUND ( 'NONE', #7946, .T. ) ;
#16212 = CARTESIAN_POINT ( 'NONE',  ( -23.00000000000002842, 10.00000000000000000, -36.99999999999999289 ) ) ;
#16213 = PLANE ( 'NONE',  #19500 ) ;
#16214 = LINE ( 'NONE', #11551, #4102 ) ;
#16215 = VECTOR ( 'NONE', #7502, 1000.000000000000000 ) ;
#16216 = EDGE_CURVE ( 'NONE', #1892, #8093, #3270, .T. ) ;
#16217 = VERTEX_POINT ( 'NONE', #19265 ) ;
#16218 = FACE_OUTER_BOUND ( 'NONE', #16887, .T. ) ;
#16219 = EDGE_LOOP ( 'NONE', ( #4660, #4242, #10696, #1131 ) ) ;
#16220 = EDGE_CURVE ( 'NONE', #17040, #16049, #19441, .T. ) ;
#16221 = CARTESIAN_POINT ( 'NONE',  ( 31.99999999999998579, 6.000000000000000000, 21.99999999999999645 ) ) ;
#16222 = ORIENTED_EDGE ( 'NONE', *, *, #16090, .F. ) ;
#16223 = CARTESIAN_POINT ( 'NONE',  ( -211.5106270998635409, 113.1299228374912502, 29.36128450348865471 ) ) ;
#16224 = AXIS2_PLACEMENT_3D ( 'NONE', #4675, #3337, #20331 ) ;
#16225 = CARTESIAN_POINT ( 'NONE',  ( 36.99999999999999289, 6.000000000000000000, 22.99999999999999645 ) ) ;
#16226 = ORIENTED_EDGE ( 'NONE', *, *, #14133, .F. ) ;
#16227 = ADVANCED_FACE ( 'NONE', ( #10089 ), #3603, .F. ) ;
#16228 = LINE ( 'NONE', #15807, #11052 ) ;
#16229 = FILL_AREA_STYLE_COLOUR ( '', #114 ) ;
#16230 = CARTESIAN_POINT ( 'NONE',  ( -22.00000000000001776, 6.000000000000000000, 32.00000000000000711 ) ) ;
#16231 = CIRCLE ( 'NONE', #16876, 10.00000000000000888 ) ;
#16232 =( NAMED_UNIT ( * ) PLANE_ANGLE_UNIT ( ) SI_UNIT ( $, .RADIAN. ) );
#16233 = DIRECTION ( 'NONE',  ( -3.328238341717372086E-14, 0.000000000000000000, 1.000000000000000000 ) ) ;
#16234 = PRESENTATION_STYLE_ASSIGNMENT (( #19190 ) ) ;
#16235 = CARTESIAN_POINT ( 'NONE',  ( -211.5106270998635409, 113.1299228374912502, 220.6387154965113382 ) ) ;
#16236 = VECTOR ( 'NONE', #11516, 1000.000000000000000 ) ;
#16237 = EDGE_LOOP ( 'NONE', ( #10316, #15061, #3889, #18948, #5328, #3544, #3842, #15126, #347, #761 ) ) ;
#16238 = CARTESIAN_POINT ( 'NONE',  ( -33.00000000000000000, 8.000000000000000000, -22.00000000000000355 ) ) ;
#16239 = DIRECTION ( 'NONE',  ( 0.000000000000000000, 1.000000000000000000, -0.000000000000000000 ) ) ;
#16240 = FILL_AREA_STYLE_COLOUR ( '', #14959 ) ;
#16241 = DIRECTION ( 'NONE',  ( 1.000000000000000000, -0.000000000000000000, 0.000000000000000000 ) ) ;
#16242 = ORIENTED_EDGE ( 'NONE', *, *, #2322, .T. ) ;
#16243 = AXIS2_PLACEMENT_3D ( 'NONE', #9367, #1830, #8141 ) ;
#16244 = VECTOR ( 'NONE', #965, 1000.000000000000000 ) ;
#16245 = EDGE_CURVE ( 'NONE', #4860, #10045, #9879, .T. ) ;
#16246 = ORIENTED_EDGE ( 'NONE', *, *, #5479, .F. ) ;
#16247 = EDGE_LOOP ( 'NONE', ( #3456, #16900, #12914, #10087 ) ) ;
#16248 = DIRECTION ( 'NONE',  ( 0.000000000000000000, 1.000000000000000000, -0.000000000000000000 ) ) ;
#16249 = VECTOR ( 'NONE', #4548, 1000.000000000000000 ) ;
#16250 = VERTEX_POINT ( 'NONE', #18505 ) ;
#16251 = EDGE_CURVE ( 'NONE', #10589, #15238, #7204, .T. ) ;
#16252 = DIRECTION ( 'NONE',  ( -1.000000000000000000, 0.000000000000000000, 0.000000000000000000 ) ) ;
#16253 = CARTESIAN_POINT ( 'NONE',  ( 1.000000000001310063, 139.7703989349544145, 489.5655098179835818 ) ) ;
#16254 = EDGE_LOOP ( 'NONE', ( #9983, #6767 ) ) ;
#16255 = DIRECTION ( 'NONE',  ( -0.000000000000000000, -0.000000000000000000, 1.000000000000000000 ) ) ;
#16256 = VECTOR ( 'NONE', #1488, 1000.000000000000000 ) ;
#16257 = VECTOR ( 'NONE', #4866, 1000.000000000000000 ) ;
#16258 =( LENGTH_UNIT ( ) NAMED_UNIT ( * ) SI_UNIT ( .MILLI., .METRE. ) );
#16259 = LINE ( 'NONE', #3769, #3147 ) ;
#16260 = SURFACE_STYLE_FILL_AREA ( #654 ) ;
#16261 = DIRECTION ( 'NONE',  ( -0.000000000000000000, -0.000000000000000000, 1.000000000000000000 ) ) ;
#16262 = EDGE_LOOP ( 'NONE', ( #10593, #3001 ) ) ;
#16263 = PLANE ( 'NONE',  #2570 ) ;
#16264 = DIRECTION ( 'NONE',  ( 0.000000000000000000, 0.000000000000000000, 1.000000000000000000 ) ) ;
#16265 = DIRECTION ( 'NONE',  ( -1.000000000000000000, 0.000000000000000000, 1.047444401652940007E-14 ) ) ;
#16266 = ORIENTED_EDGE ( 'NONE', *, *, #2560, .T. ) ;
#16267 = CARTESIAN_POINT ( 'NONE',  ( -40.00000000000000000, 0.000000000000000000, 26.00000000000000355 ) ) ;
#16268 = CARTESIAN_POINT ( 'NONE',  ( -1.336826079150933300E-12, 139.7703989349544145, 489.5655098179848892 ) ) ;
#16269 = VERTEX_POINT ( 'NONE', #16696 ) ;
#16270 = EDGE_LOOP ( 'NONE', ( #7536, #1578, #9167, #6491 ) ) ;
#16271 = VECTOR ( 'NONE', #10780, 1000.000000000000000 ) ;
#16272 = AXIS2_PLACEMENT_3D ( 'NONE', #6971, #16554, #10248 ) ;
#16273 = ORIENTED_EDGE ( 'NONE', *, *, #16339, .T. ) ;
#16274 =( NAMED_UNIT ( * ) SI_UNIT ( $, .STERADIAN. ) SOLID_ANGLE_UNIT ( ) );
#16275 = CARTESIAN_POINT ( 'NONE',  ( -22.00000000000001776, 6.000000000000000000, 36.00000000000000711 ) ) ;
#16276 = VERTEX_POINT ( 'NONE', #15438 ) ;
#16277 = CARTESIAN_POINT ( 'NONE',  ( 40.00000000000000711, 19.00000000000000000, 25.99999999999999645 ) ) ;
#16278 = VECTOR ( 'NONE', #4062, 1000.000000000000000 ) ;
#16279 = ADVANCED_FACE ( 'NONE', ( #20042 ), #11936, .T. ) ;
#16280 = VECTOR ( 'NONE', #10518, 1000.000000000000000 ) ;
#16281 = ORIENTED_EDGE ( 'NONE', *, *, #14401, .T. ) ;
#16282 = DIRECTION ( 'NONE',  ( -1.000000000000000000, -0.000000000000000000, -0.000000000000000000 ) ) ;
#16283 = COLOUR_RGB ( '', 0.66274510, 0.83137255, 0.94901961) ;
#16284 = CARTESIAN_POINT ( 'NONE',  ( -25.99999999999999645, 68.00000000000000000, 40.00000000000002132 ) ) ;
#16285 = CARTESIAN_POINT ( 'NONE',  ( 0.3790268517283566507, 139.8046609698958775, 489.3602998400258457 ) ) ;
#16286 = CARTESIAN_POINT ( 'NONE',  ( 423.8334540492694487, 191.8198460455371333, 81.76606011801540319 ) ) ;
#16287 = DIRECTION ( 'NONE',  ( 1.000000000000000000, 0.000000000000000000, 0.000000000000000000 ) ) ;
#16288 = CIRCLE ( 'NONE', #6075, 17.85000000000000142 ) ;
#16290 = VECTOR ( 'NONE', #1230, 1000.000000000000000 ) ;
#16289 = CYLINDRICAL_SURFACE ( 'NONE', #11029, 4.999999999999997335 ) ;
#16291 = DIRECTION ( 'NONE',  ( -0.000000000000000000, -1.000000000000000000, -0.000000000000000000 ) ) ;
#16292 = CIRCLE ( 'NONE', #6407, 1.000000000000000888 ) ;
#16293 = EDGE_LOOP ( 'NONE', ( #20358, #17804, #10975, #11658 ) ) ;
#16294 = CARTESIAN_POINT ( 'NONE',  ( -31.81980515339462912, 8.000000000000000000, -31.81980515339465043 ) ) ;
#16295 = LINE ( 'NONE', #14928, #12157 ) ;
#16296 = EDGE_LOOP ( 'NONE', ( #9318, #7914, #18569, #7985 ) ) ;
#16297 = AXIS2_PLACEMENT_3D ( 'NONE', #16491, #2345, #8643 ) ;
#16298 = ORIENTED_EDGE ( 'NONE', *, *, #4688, .F. ) ;
#16299 = COLOUR_RGB ( '', 0.40784314, 0.44705882, 0.49803922) ;
#16300 = EDGE_CURVE ( 'NONE', #3638, #17811, #7503, .T. ) ;
#16301 = ORIENTED_EDGE ( 'NONE', *, *, #9833, .F. ) ;
#16302 = ORIENTED_EDGE ( 'NONE', *, *, #1528, .T. ) ;
#16303 = ORIENTED_EDGE ( 'NONE', *, *, #3671, .T. ) ;
#16304 = STYLED_ITEM ( 'NONE', ( #52 ), #12428 ) ;
#16305 = CONICAL_SURFACE ( 'NONE', #3779, 13.62500000000000000, 0.2281026282799422378 ) ;
#16306 = DIRECTION ( 'NONE',  ( 6.152690941188070202E-17, -0.6268583551835633649, 0.7791332379872890623 ) ) ;
#16307 = AXIS2_PLACEMENT_3D ( 'NONE', #2358, #13214, #5564 ) ;
#16308 = DIRECTION ( 'NONE',  ( 0.000000000000000000, 0.000000000000000000, -1.000000000000000000 ) ) ;
#16309 = DIRECTION ( 'NONE',  ( 1.000000000000000000, 0.000000000000000000, 0.000000000000000000 ) ) ;
#16310 = VECTOR ( 'NONE', #19884, 1000.000000000000000 ) ;
#16311 = CARTESIAN_POINT ( 'NONE',  ( -44.50085094405409336, 193.0431417881923153, 505.3921618609452935 ) ) ;
#16313 = EDGE_CURVE ( 'NONE', #6685, #17182, #18095, .T. ) ;
#16312 = DIRECTION ( 'NONE',  ( -0.000000000000000000, -1.000000000000000000, -0.000000000000000000 ) ) ;
#16314 = CIRCLE ( 'NONE', #10040, 1.000000000000000888 ) ;
#16315 = PLANE ( 'NONE',  #13734 ) ;
#16316 =( GEOMETRIC_REPRESENTATION_CONTEXT ( 3 ) GLOBAL_UNCERTAINTY_ASSIGNED_CONTEXT ( ( #18061 ) ) GLOBAL_UNIT_ASSIGNED_CONTEXT ( ( #2012, #4837, #14305 ) ) REPRESENTATION_CONTEXT ( 'NONE', 'WORKASPACE' ) );
#16317 = LINE ( 'NONE', #10106, #2652 ) ;
#16318 = EDGE_CURVE ( 'NONE', #17762, #14156, #18203, .T. ) ;
#16319 = DIRECTION ( 'NONE',  ( -0.000000000000000000, -1.000000000000000000, -0.000000000000000000 ) ) ;
#16320 = AXIS2_PLACEMENT_3D ( 'NONE', #12726, #11469, #17752 ) ;
#16321 = LINE ( 'NONE', #3725, #9034 ) ;
#16322 = VECTOR ( 'NONE', #13459, 1000.000000000000000 ) ;
#16323 = ORIENTED_EDGE ( 'NONE', *, *, #7097, .T. ) ;
#16324 = AXIS2_PLACEMENT_3D ( 'NONE', #11966, #2365, #13718 ) ;
#16325 = CIRCLE ( 'NONE', #6725, 10.00000000000000178 ) ;
#16326 = SURFACE_STYLE_FILL_AREA ( #6626 ) ;
#16327 = UNCERTAINTY_MEASURE_WITH_UNIT (LENGTH_MEASURE( 1.000000000000000082E-05 ), #17609, 'distance_accuracy_value', 'NONE');
#16328 = ORIENTED_EDGE ( 'NONE', *, *, #6858, .F. ) ;
#16329 = EDGE_CURVE ( 'NONE', #19900, #3196, #2748, .T. ) ;
#16330 = VECTOR ( 'NONE', #16148, 1000.000000000000000 ) ;
#16331 = VERTEX_POINT ( 'NONE', #4110 ) ;
#16332 = CARTESIAN_POINT ( 'NONE',  ( 37.00000000000000000, 0.000000000000000000, 23.00000000000001066 ) ) ;
#16333 = UNCERTAINTY_MEASURE_WITH_UNIT (LENGTH_MEASURE( 1.000000000000000082E-05 ), #6563, 'distance_accuracy_value', 'NONE');
#16334 = FACE_OUTER_BOUND ( 'NONE', #2532, .T. ) ;
#16335 = CARTESIAN_POINT ( 'NONE',  ( -78.99999999999995737, 146.8256012863087108, 507.0490161104376057 ) ) ;
#16336 = EDGE_LOOP ( 'NONE', ( #9647, #3056, #16172, #6670 ) ) ;
#16337 = VECTOR ( 'NONE', #11676, 1000.000000000000000 ) ;
#16339 = EDGE_CURVE ( 'NONE', #11965, #10871, #9141, .T. ) ;
#16338 = DIRECTION ( 'NONE',  ( 1.000000000000000000, 5.889072920838430686E-16, 0.000000000000000000 ) ) ;
#16340 = PRESENTATION_STYLE_ASSIGNMENT (( #11467 ) ) ;
#16341 =( GEOMETRIC_REPRESENTATION_CONTEXT ( 3 ) GLOBAL_UNCERTAINTY_ASSIGNED_CONTEXT ( ( #9917 ) ) GLOBAL_UNIT_ASSIGNED_CONTEXT ( ( #7237, #2171, #19773 ) ) REPRESENTATION_CONTEXT ( 'NONE', 'WORKASPACE' ) );
#16342 = CYLINDRICAL_SURFACE ( 'NONE', #15841, 3.299999999999997158 ) ;
#16343 = CARTESIAN_POINT ( 'NONE',  ( 463.8334540492693350, 191.8198460455371333, 34.99421986894476788 ) ) ;
#16344 = EDGE_CURVE ( 'NONE', #5100, #18923, #9044, .T. ) ;
#16345 = ORIENTED_EDGE ( 'NONE', *, *, #6887, .T. ) ;
#16346 = LINE ( 'NONE', #12933, #4253 ) ;
#16347 = DIRECTION ( 'NONE',  ( -0.000000000000000000, -1.000000000000000000, 0.000000000000000000 ) ) ;
#16348 = CIRCLE ( 'NONE', #14334, 3.000000000000002665 ) ;
#16349 = EDGE_CURVE ( 'NONE', #4111, #10206, #13773, .T. ) ;
#16350 = EDGE_CURVE ( 'NONE', #4262, #9522, #9204, .T. ) ;
#16351 = ORIENTED_EDGE ( 'NONE', *, *, #10744, .T. ) ;
#16352 = EDGE_CURVE ( 'NONE', #11636, #16176, #19945, .T. ) ;
#16353 = ORIENTED_EDGE ( 'NONE', *, *, #4099, .F. ) ;
#16354 = AXIS2_PLACEMENT_3D ( 'NONE', #1115, #2787, #19986 ) ;
#16355 = CARTESIAN_POINT ( 'NONE',  ( -34.99999999999998579, 3.000000000000000000, 21.00000000000000355 ) ) ;
#16356 = EDGE_LOOP ( 'NONE', ( #3318, #14174, #14208, #12013 ) ) ;
#16357 = CARTESIAN_POINT ( 'NONE',  ( 2.844883903241205214, 40.02776846313489045, 9.064373830433188672 ) ) ;
#16358 = VERTEX_POINT ( 'NONE', #885 ) ;
#16359 = PRESENTATION_STYLE_ASSIGNMENT (( #13153 ) ) ;
#16360 = DIRECTION ( 'NONE',  ( -0.000000000000000000, -0.000000000000000000, 1.000000000000000000 ) ) ;
#16361 =( NAMED_UNIT ( * ) PLANE_ANGLE_UNIT ( ) SI_UNIT ( $, .RADIAN. ) );
#16362 = AXIS2_PLACEMENT_3D ( 'NONE', #2466, #10409, #9066 ) ;
#16363 = FILL_AREA_STYLE_COLOUR ( '', #1927 ) ;
#16364 = LINE ( 'NONE', #564, #11673 ) ;
#16365 = ORIENTED_EDGE ( 'NONE', *, *, #18334, .F. ) ;
#16366 = LINE ( 'NONE', #8492, #10526 ) ;
#16367 = DIRECTION ( 'NONE',  ( 0.000000000000000000, 0.000000000000000000, -1.000000000000000000 ) ) ;
#16368 = DIRECTION ( 'NONE',  ( 0.000000000000000000, 1.000000000000000000, 1.632680918566406793E-16 ) ) ;
#16369 = CARTESIAN_POINT ( 'NONE',  ( 463.8334540492693350, 134.2156642432025251, -87.31255586191144857 ) ) ;
#16370 = PLANE ( 'NONE',  #12626 ) ;
#16371 =( GEOMETRIC_REPRESENTATION_CONTEXT ( 3 ) GLOBAL_UNCERTAINTY_ASSIGNED_CONTEXT ( ( #16126 ) ) GLOBAL_UNIT_ASSIGNED_CONTEXT ( ( #20166, #7718, #1707 ) ) REPRESENTATION_CONTEXT ( 'NONE', 'WORKASPACE' ) );
#16372 = CARTESIAN_POINT ( 'NONE',  ( 0.9999999999999872324, 216.7545334744432921, 488.5655098179835818 ) ) ;
#16373 = EDGE_CURVE ( 'NONE', #6211, #3049, #12132, .T. ) ;
#16374 = ORIENTED_EDGE ( 'NONE', *, *, #19666, .F. ) ;
#16375 = AXIS2_PLACEMENT_3D ( 'NONE', #11536, #13301, #11849 ) ;
#16376 = ADVANCED_FACE ( 'NONE', ( #5546 ), #15032, .F. ) ;
#16377 = ORIENTED_EDGE ( 'NONE', *, *, #4220, .T. ) ;
#16378 = EDGE_CURVE ( 'NONE', #2143, #9868, #4276, .T. ) ;
#16379 = EDGE_LOOP ( 'NONE', ( #6340, #5383, #7647, #929 ) ) ;
#16380 = ORIENTED_EDGE ( 'NONE', *, *, #10779, .T. ) ;
#16381 = LINE ( 'NONE', #16077, #2349 ) ;
#16382 = CARTESIAN_POINT ( 'NONE',  ( -1.000000000000011768, 142.0976792249508946, 502.3210940490797611 ) ) ;
#16383 = ORIENTED_EDGE ( 'NONE', *, *, #2921, .T. ) ;
#16384 = EDGE_LOOP ( 'NONE', ( #245, #17097 ) ) ;
#16385 = CARTESIAN_POINT ( 'NONE',  ( 111.4893729001366154, 77.72476844875745883, 252.0000000000000000 ) ) ;
#16386 = DIRECTION ( 'NONE',  ( -0.000000000000000000, -1.000000000000000000, -0.000000000000000000 ) ) ;
#16387 = CARTESIAN_POINT ( 'NONE',  ( -1.000000000000013101, 139.2066006846527841, 488.2525619656395861 ) ) ;
#16388 = LINE ( 'NONE', #5244, #5400 ) ;
#16389 = CARTESIAN_POINT ( 'NONE',  ( -34.99999999999998579, 0.000000000000000000, 21.00000000000000355 ) ) ;
#16390 = CARTESIAN_POINT ( 'NONE',  ( -36.99999999999997868, 0.000000000000000000, -19.99999999999999289 ) ) ;
#16391 = CARTESIAN_POINT ( 'NONE',  ( 37.00000000000003553, 0.000000000000000000, 23.00000000000000355 ) ) ;
#16392 = FACE_OUTER_BOUND ( 'NONE', #9407, .T. ) ;
#16393 = VERTEX_POINT ( 'NONE', #17076 ) ;
#16394 = SURFACE_STYLE_FILL_AREA ( #16094 ) ;
#16395 = SURFACE_SIDE_STYLE ('',( #1918 ) ) ;
#16396 = ORIENTED_EDGE ( 'NONE', *, *, #12163, .F. ) ;
#16397 = ADVANCED_FACE ( 'NONE', ( #14284 ), #9540, .F. ) ;
#16398 = ORIENTED_EDGE ( 'NONE', *, *, #12498, .T. ) ;
#16399 = ORIENTED_EDGE ( 'NONE', *, *, #19709, .T. ) ;
#16400 = EDGE_LOOP ( 'NONE', ( #12020, #13378, #14661, #18730 ) ) ;
#16401 = ORIENTED_EDGE ( 'NONE', *, *, #2312, .F. ) ;
#16402 = SURFACE_STYLE_FILL_AREA ( #695 ) ;
#16403 = FACE_OUTER_BOUND ( 'NONE', #18967, .T. ) ;
#16404 = DIRECTION ( 'NONE',  ( 1.000000000000000000, 0.000000000000000000, 0.000000000000000000 ) ) ;
#16405 = DIRECTION ( 'NONE',  ( 0.000000000000000000, 1.000000000000000000, -0.000000000000000000 ) ) ;
#16406 = AXIS2_PLACEMENT_3D ( 'NONE', #15401, #1231, #20226 ) ;
#16407 = SURFACE_STYLE_USAGE ( .BOTH. , #5365 ) ;
#16408 = FILL_AREA_STYLE_COLOUR ( '', #13611 ) ;
#16409 = CIRCLE ( 'NONE', #5527, 18.50000000000000000 ) ;
#16410 = DIRECTION ( 'NONE',  ( 1.000000000000000000, 6.123031769111888756E-17, 7.900838015626929923E-17 ) ) ;
#16411 = LINE ( 'NONE', #14359, #18762 ) ;
#16412 = FACE_OUTER_BOUND ( 'NONE', #11090, .T. ) ;
#16413 = DIRECTION ( 'NONE',  ( 0.000000000000000000, 0.000000000000000000, -1.000000000000000000 ) ) ;
#16414 = DIRECTION ( 'NONE',  ( 0.000000000000000000, 0.000000000000000000, -1.000000000000000000 ) ) ;
#16415 = EDGE_LOOP ( 'NONE', ( #1717, #2234, #19619, #14417 ) ) ;
#16416 = ORIENTED_EDGE ( 'NONE', *, *, #17702, .F. ) ;
#16417 = VECTOR ( 'NONE', #7801, 1000.000000000000000 ) ;
#16418 = CARTESIAN_POINT ( 'NONE',  ( -22.00000000000001776, 8.000000000000000000, 33.00000000000000711 ) ) ;
#16419 = ORIENTED_EDGE ( 'NONE', *, *, #15161, .T. ) ;
#16420 = ORIENTED_EDGE ( 'NONE', *, *, #5067, .T. ) ;
#16421 = DIRECTION ( 'NONE',  ( 1.000000000000000000, 0.000000000000000000, 0.000000000000000000 ) ) ;
#16422 = DIRECTION ( 'NONE',  ( 0.000000000000000000, 0.000000000000000000, 1.000000000000000000 ) ) ;
#16423 = VERTEX_POINT ( 'NONE', #9340 ) ;
#16424 = CARTESIAN_POINT ( 'NONE',  ( 55.98937290013660828, 95.58236431990633264, 327.6194023385999685 ) ) ;
#16425 = LINE ( 'NONE', #5577, #18240 ) ;
#16426 = PLANE ( 'NONE',  #14577 ) ;
#16427 = EDGE_CURVE ( 'NONE', #4190, #15899, #958, .T. ) ;
#16428 = DIRECTION ( 'NONE',  ( 0.000000000000000000, 0.000000000000000000, 1.000000000000000000 ) ) ;
#16429 = CARTESIAN_POINT ( 'NONE',  ( -211.5106270998635409, 123.1299228374912644, 29.36128450348865471 ) ) ;
#16430 = LINE ( 'NONE', #2268, #12350 ) ;
#16431 = COLOUR_RGB ( '', 0.09019608, 0.27058824, 0.51372549) ;
#16432 = ORIENTED_EDGE ( 'NONE', *, *, #7894, .F. ) ;
#16433 = CARTESIAN_POINT ( 'NONE',  ( -31.81980515339462912, 0.000000000000000000, 31.81980515339465043 ) ) ;
#16434 = DIRECTION ( 'NONE',  ( 0.000000000000000000, 1.000000000000000000, 0.000000000000000000 ) ) ;
#16435 = ADVANCED_FACE ( 'NONE', ( #169 ), #18714, .F. ) ;
#16436 = EDGE_LOOP ( 'NONE', ( #9653, #14885, #18012, #10442 ) ) ;
#16437 = ORIENTED_EDGE ( 'NONE', *, *, #1668, .T. ) ;
#16438 = EDGE_CURVE ( 'NONE', #12058, #17253, #1373, .T. ) ;
#16440 = ORIENTED_EDGE ( 'NONE', *, *, #12835, .F. ) ;
#16439 = VECTOR ( 'NONE', #13460, 1000.000000000000000 ) ;
#16441 = DIRECTION ( 'NONE',  ( 0.000000000000000000, 0.000000000000000000, -1.000000000000000000 ) ) ;
#16442 = DIRECTION ( 'NONE',  ( -0.000000000000000000, -1.000000000000000000, -0.000000000000000000 ) ) ;
#16443 = ORIENTED_EDGE ( 'NONE', *, *, #8400, .F. ) ;
#16444 = EDGE_CURVE ( 'NONE', #14898, #3610, #7900, .T. ) ;
#16445 = LINE ( 'NONE', #17562, #7741 ) ;
#16446 = CARTESIAN_POINT ( 'NONE',  ( -211.5106270998635409, 113.1299228374912502, 79.58252780074349175 ) ) ;
#16447 = UNCERTAINTY_MEASURE_WITH_UNIT (LENGTH_MEASURE( 1.000000000000000082E-05 ), #8201, 'distance_accuracy_value', 'NONE');
#16448 =( LENGTH_UNIT ( ) NAMED_UNIT ( * ) SI_UNIT ( .MILLI., .METRE. ) );
#16449 = DIRECTION ( 'NONE',  ( 0.000000000000000000, 0.000000000000000000, 1.000000000000000000 ) ) ;
#16450 = ORIENTED_EDGE ( 'NONE', *, *, #9470, .F. ) ;
#16451 = CARTESIAN_POINT ( 'NONE',  ( -1.000000000000001110, 138.7545334744432637, 478.3411705753777596 ) ) ;
#16452 = ADVANCED_FACE ( 'NONE', ( #18623 ), #2945, .T. ) ;
#16453 = CARTESIAN_POINT ( 'NONE',  ( -64.99999999999995737, 317.7545334744432353, 495.1946179577816451 ) ) ;
#16454 = FACE_OUTER_BOUND ( 'NONE', #5433, .T. ) ;
#16455 = CARTESIAN_POINT ( 'NONE',  ( -33.00000000000000000, 8.000000000000000000, -26.00000000000000355 ) ) ;
#16456 = PRESENTATION_LAYER_ASSIGNMENT (  '', '', ( #4922 ) ) ;
#16457 = AXIS2_PLACEMENT_3D ( 'NONE', #11799, #13644, #937 ) ;
#16458 = CARTESIAN_POINT ( 'NONE',  ( 21.99999999999998224, 6.000000000000000000, -35.99999999999999289 ) ) ;
#16459 = MECHANICAL_DESIGN_GEOMETRIC_PRESENTATION_REPRESENTATION (  '', ( #311 ), #1596 ) ;
#16460 = ORIENTED_EDGE ( 'NONE', *, *, #16964, .F. ) ;
#16461 = VERTEX_POINT ( 'NONE', #9854 ) ;
#16462 = EDGE_CURVE ( 'NONE', #258, #7981, #19117, .T. ) ;
#16463 = EDGE_LOOP ( 'NONE', ( #11573, #763, #12230, #113 ) ) ;
#16464 = ORIENTED_EDGE ( 'NONE', *, *, #20106, .T. ) ;
#16465 = ORIENTED_EDGE ( 'NONE', *, *, #7379, .T. ) ;
#16466 = LINE ( 'NONE', #1443, #376 ) ;
#16467 = DIRECTION ( 'NONE',  ( 0.000000000000000000, -1.000000000000000000, 0.000000000000000000 ) ) ;
#16468 = ORIENTED_EDGE ( 'NONE', *, *, #8262, .T. ) ;
#16469 = EDGE_CURVE ( 'NONE', #15549, #1444, #6790, .T. ) ;
#16470 = VECTOR ( 'NONE', #16683, 1000.000000000000000 ) ;
#16471 = FACE_OUTER_BOUND ( 'NONE', #16400, .T. ) ;
#16472 =( NAMED_UNIT ( * ) PLANE_ANGLE_UNIT ( ) SI_UNIT ( $, .RADIAN. ) );
#16473 = LINE ( 'NONE', #8831, #16470 ) ;
#16474 = CARTESIAN_POINT ( 'NONE',  ( -23.00000000000002132, 0.000000000000000000, 37.00000000000000711 ) ) ;
#16475 = EDGE_CURVE ( 'NONE', #15985, #7546, #361, .T. ) ;
#16476 = CARTESIAN_POINT ( 'NONE',  ( -0.8056780331109345550, 138.9431362660446609, 489.2309999112469541 ) ) ;
#16477 = DIRECTION ( 'NONE',  ( 1.000000000000000000, -0.000000000000000000, 0.000000000000000000 ) ) ;
#16478 = DIRECTION ( 'NONE',  ( -1.000000000000000000, 0.000000000000000000, 0.000000000000000000 ) ) ;
#16479 = CARTESIAN_POINT ( 'NONE',  ( 493.8117674897343363, 134.2156642432025251, 250.0000000000000000 ) ) ;
#16480 = FACE_OUTER_BOUND ( 'NONE', #14023, .T. ) ;
#16481 = VERTEX_POINT ( 'NONE', #8425 ) ;
#16482 = MECHANICAL_DESIGN_GEOMETRIC_PRESENTATION_REPRESENTATION (  '', ( #18422 ), #19083 ) ;
#16483 = AXIS2_PLACEMENT_3D ( 'NONE', #7864, #20228, #6227 ) ;
#16484 = EDGE_LOOP ( 'NONE', ( #1767, #5526, #2086, #4023, #1130 ) ) ;
#16485 = UNCERTAINTY_MEASURE_WITH_UNIT (LENGTH_MEASURE( 1.000000000000000082E-05 ), #17685, 'distance_accuracy_value', 'NONE');
#16486 = ORIENTED_EDGE ( 'NONE', *, *, #2707, .F. ) ;
#16488 = ORIENTED_EDGE ( 'NONE', *, *, #10734, .T. ) ;
#16487 = ADVANCED_FACE ( 'NONE', ( #19237 ), #9759, .F. ) ;
#16489 = EDGE_LOOP ( 'NONE', ( #14058, #6798, #13559, #4639 ) ) ;
#16490 =( NAMED_UNIT ( * ) PLANE_ANGLE_UNIT ( ) SI_UNIT ( $, .RADIAN. ) );
#16491 = CARTESIAN_POINT ( 'NONE',  ( 21.99999999999998224, 8.000000000000000000, -35.99999999999999289 ) ) ;
#16492 = DIRECTION ( 'NONE',  ( 1.000000000000000000, 9.815121534730717399E-17, -0.000000000000000000 ) ) ;
#16493 = LINE ( 'NONE', #6824, #4402 ) ;
#16494 = DIRECTION ( 'NONE',  ( 0.000000000000000000, 1.000000000000000000, 0.000000000000000000 ) ) ;
#16495 = AXIS2_PLACEMENT_3D ( 'NONE', #8084, #18981, #237 ) ;
#16496 = CARTESIAN_POINT ( 'NONE',  ( -80.99999999999995737, 138.7545334744432637, 488.5655098179835818 ) ) ;
#16497 = VECTOR ( 'NONE', #19288, 1000.000000000000000 ) ;
#16498 = AXIS2_PLACEMENT_3D ( 'NONE', #11431, #7003, #13291 ) ;
#16499 = DIRECTION ( 'NONE',  ( -1.314570224013242627E-15, 1.000000000000000000, 0.000000000000000000 ) ) ;
#16500 = CARTESIAN_POINT ( 'NONE',  ( 153.4893729001366864, 113.1299228374914634, 29.36128450348865471 ) ) ;
#16501 =( NAMED_UNIT ( * ) PLANE_ANGLE_UNIT ( ) SI_UNIT ( $, .RADIAN. ) );
#16502 = DIRECTION ( 'NONE',  ( 0.000000000000000000, 0.000000000000000000, -1.000000000000000000 ) ) ;
#16503 = DIRECTION ( 'NONE',  ( -1.000000000000000000, 0.000000000000000000, 0.000000000000000000 ) ) ;
#16504 = CARTESIAN_POINT ( 'NONE',  ( 2.181929469892549545, 139.7545334744432637, 491.0690926367355473 ) ) ;
#16505 =( GEOMETRIC_REPRESENTATION_CONTEXT ( 3 ) GLOBAL_UNCERTAINTY_ASSIGNED_CONTEXT ( ( #7929 ) ) GLOBAL_UNIT_ASSIGNED_CONTEXT ( ( #12701, #1532, #13925 ) ) REPRESENTATION_CONTEXT ( 'NONE', 'WORKASPACE' ) );
#16506 = DIRECTION ( 'NONE',  ( -1.000000000000000000, 0.000000000000000000, 0.000000000000000000 ) ) ;
#16507 = CARTESIAN_POINT ( 'NONE',  ( 0.000000000000000000, 0.000000000000000000, 250.0000000000000000 ) ) ;
#16508 = ORIENTED_EDGE ( 'NONE', *, *, #2145, .T. ) ;
#16509 = VECTOR ( 'NONE', #9533, 1000.000000000000000 ) ;
#16510 = VECTOR ( 'NONE', #6488, 1000.000000000000000 ) ;
#16511 = CIRCLE ( 'NONE', #18456, 10.00000000000000888 ) ;
#16512 = VERTEX_POINT ( 'NONE', #8318 ) ;
#16513 = PRESENTATION_STYLE_ASSIGNMENT (( #3922 ) ) ;
#16514 = UNCERTAINTY_MEASURE_WITH_UNIT (LENGTH_MEASURE( 1.000000000000000082E-05 ), #11193, 'distance_accuracy_value', 'NONE');
#16515 = ORIENTED_EDGE ( 'NONE', *, *, #7227, .F. ) ;
#16516 = ORIENTED_EDGE ( 'NONE', *, *, #8255, .F. ) ;
#16517 = EDGE_LOOP ( 'NONE', ( #4257, #17147, #17831, #8962 ) ) ;
#16518 = DIRECTION ( 'NONE',  ( 0.000000000000000000, -0.000000000000000000, -1.000000000000000000 ) ) ;
#16519 = UNCERTAINTY_MEASURE_WITH_UNIT (LENGTH_MEASURE( 1.000000000000000082E-05 ), #13685, 'distance_accuracy_value', 'NONE');
#16520 = EDGE_LOOP ( 'NONE', ( #4536, #13319, #17328, #14564 ) ) ;
#16521 = CARTESIAN_POINT ( 'NONE',  ( -1.776356839400249676E-15, 0.000000000000000000, 0.000000000000000000 ) ) ;
#16522 = DIRECTION ( 'NONE',  ( 1.000000000000000000, 0.000000000000000000, 1.322948291343119651E-12 ) ) ;
#16523 = EDGE_CURVE ( 'NONE', #3146, #13356, #13083, .T. ) ;
#16524 = CARTESIAN_POINT ( 'NONE',  ( 3.500000000000000000, 0.000000000000000000, 0.000000000000000000 ) ) ;
#16525 = VECTOR ( 'NONE', #17378, 1000.000000000000227 ) ;
#16526 = DIRECTION ( 'NONE',  ( 1.000000000000000000, 9.815121534730717399E-17, -0.000000000000000000 ) ) ;
#16527 = CARTESIAN_POINT ( 'NONE',  ( 0.000000000000000000, 0.000000000000000000, -150.0000000000000000 ) ) ;
#16528 = LINE ( 'NONE', #11782, #19738 ) ;
#16529 = CYLINDRICAL_SURFACE ( 'NONE', #13355, 4.999999999999997335 ) ;
#16530 = VERTEX_POINT ( 'NONE', #8948 ) ;
#16531 = CARTESIAN_POINT ( 'NONE',  ( 35.00000000000003553, -20.00000000000000000, -20.99999999999999645 ) ) ;
#16532 = CARTESIAN_POINT ( 'NONE',  ( 153.4893729001366580, 0.000000000000000000, 0.000000000000000000 ) ) ;
#16533 = EDGE_CURVE ( 'NONE', #2216, #5003, #5919, .T. ) ;
#16534 = VERTEX_POINT ( 'NONE', #9070 ) ;
#16535 = AXIS2_PLACEMENT_3D ( 'NONE', #9317, #3144, #20123 ) ;
#16536 = AXIS2_PLACEMENT_3D ( 'NONE', #371, #14712, #3491 ) ;
#16537 = ORIENTED_EDGE ( 'NONE', *, *, #7724, .F. ) ;
#16538 = DIRECTION ( 'NONE',  ( 1.000000000000000000, 0.000000000000000000, 0.000000000000000000 ) ) ;
#16539 = DIRECTION ( 'NONE',  ( -5.551115123125782071E-14, 1.203706215242021147E-29, -1.000000000000000000 ) ) ;
#16540 = UNCERTAINTY_MEASURE_WITH_UNIT (LENGTH_MEASURE( 1.000000000000000082E-05 ), #19040, 'distance_accuracy_value', 'NONE');
#16541 = ORIENTED_EDGE ( 'NONE', *, *, #7976, .T. ) ;
#16542 = CYLINDRICAL_SURFACE ( 'NONE', #8224, 2.500000000000002220 ) ;
#16543 = CARTESIAN_POINT ( 'NONE',  ( -80.25208250843274982, 139.5548694108364316, 500.3753056083104411 ) ) ;
#16544 = AXIS2_PLACEMENT_3D ( 'NONE', #14893, #5426, #11402 ) ;
#16545 = DIRECTION ( 'NONE',  ( -0.000000000000000000, 1.000000000000000000, -0.000000000000000000 ) ) ;
#16546 =( LENGTH_UNIT ( ) NAMED_UNIT ( * ) SI_UNIT ( .MILLI., .METRE. ) );
#16547 = ADVANCED_FACE ( 'NONE', ( #10601 ), #10501, .F. ) ;
#16548 = LINE ( 'NONE', #18279, #1434 ) ;
#16549 = ORIENTED_EDGE ( 'NONE', *, *, #1932, .T. ) ;
#16550 = CARTESIAN_POINT ( 'NONE',  ( 30.99999999999995737, 0.000000000000000000, 31.00000000000000000 ) ) ;
#16551 = CARTESIAN_POINT ( 'NONE',  ( 0.000000000000000000, 316.7545334744432921, 155.1946179577816167 ) ) ;
#16552 = CIRCLE ( 'NONE', #2035, 10.00000000000000888 ) ;
#16553 = AXIS2_PLACEMENT_3D ( 'NONE', #17373, #7589, #18616 ) ;
#16554 = DIRECTION ( 'NONE',  ( -0.000000000000000000, 1.000000000000000000, -0.000000000000000000 ) ) ;
#16555 = CARTESIAN_POINT ( 'NONE',  ( 33.49999999999839417, -18.32650529562336672, 176.5415023676507076 ) ) ;
#16556 = ORIENTED_EDGE ( 'NONE', *, *, #17198, .T. ) ;
#16557 = ADVANCED_FACE ( 'NONE', ( #5877 ), #2866, .F. ) ;
#16558 = SURFACE_STYLE_USAGE ( .BOTH. , #7484 ) ;
#16559 = ORIENTED_EDGE ( 'NONE', *, *, #7729, .F. ) ;
#16560 = ORIENTED_EDGE ( 'NONE', *, *, #16735, .F. ) ;
#16561 = PRODUCT_DEFINITION_FORMATION_WITH_SPECIFIED_SOURCE ( 'ANY', '', #12546, .NOT_KNOWN. ) ;
#16562 =( GEOMETRIC_REPRESENTATION_CONTEXT ( 3 ) GLOBAL_UNCERTAINTY_ASSIGNED_CONTEXT ( ( #13063 ) ) GLOBAL_UNIT_ASSIGNED_CONTEXT ( ( #16258, #16734, #6666 ) ) REPRESENTATION_CONTEXT ( 'NONE', 'WORKASPACE' ) );
#16563 = VECTOR ( 'NONE', #16233, 1000.000000000000000 ) ;
#16564 = EDGE_LOOP ( 'NONE', ( #7282, #14672, #10652, #11600 ) ) ;
#16565 = EDGE_CURVE ( 'NONE', #10095, #3482, #18328, .T. ) ;
#16566 = VERTEX_POINT ( 'NONE', #5561 ) ;
#16567 = CARTESIAN_POINT ( 'NONE',  ( 10.00000000000000000, 309.2289037985890445, -143.5198051533984085 ) ) ;
#16568 = EDGE_CURVE ( 'NONE', #8069, #13882, #11859, .T. ) ;
#16569 = AXIS2_PLACEMENT_3D ( 'NONE', #15755, #18712, #18916 ) ;
#16570 = DIRECTION ( 'NONE',  ( 3.328238341717372086E-14, 0.000000000000000000, -1.000000000000000000 ) ) ;
#16571 = AXIS2_PLACEMENT_3D ( 'NONE', #15336, #18710, #15542 ) ;
#16572 = ORIENTED_EDGE ( 'NONE', *, *, #467, .F. ) ;
#16573 = DIRECTION ( 'NONE',  ( 0.000000000000000000, -1.000000000000000000, 0.000000000000000000 ) ) ;
#16574 = FACE_OUTER_BOUND ( 'NONE', #9763, .T. ) ;
#16575 = DIRECTION ( 'NONE',  ( -1.000000000000000000, -0.000000000000000000, -0.000000000000000000 ) ) ;
#16576 = CARTESIAN_POINT ( 'NONE',  ( -20.99999999999999645, 19.00000000000000000, -31.00000000000003908 ) ) ;
#16577 = CARTESIAN_POINT ( 'NONE',  ( 0.000000000000000000, 3.000000000000000888, -150.0000000000000000 ) ) ;
#16578 = EDGE_CURVE ( 'NONE', #11216, #12891, #5661, .T. ) ;
#16579 = SURFACE_SIDE_STYLE ('',( #2636 ) ) ;
#16580 = PRESENTATION_LAYER_ASSIGNMENT (  '', '', ( #2392 ) ) ;
#16581 = AXIS2_PLACEMENT_3D ( 'NONE', #4840, #18937, #4730 ) ;
#16582 = LINE ( 'NONE', #8522, #14413 ) ;
#16583 = DIRECTION ( 'NONE',  ( 0.000000000000000000, -0.000000000000000000, -1.000000000000000000 ) ) ;
#16584 = CARTESIAN_POINT ( 'NONE',  ( 31.00000000000001421, 10.00000000000000000, 22.99999999999999645 ) ) ;
#16585 = DIRECTION ( 'NONE',  ( -0.000000000000000000, 0.000000000000000000, 1.000000000000000000 ) ) ;
#16586 = DIRECTION ( 'NONE',  ( 1.000000000000000000, 0.000000000000000000, -0.000000000000000000 ) ) ;
#16587 = FACE_OUTER_BOUND ( 'NONE', #11304, .T. ) ;
#16588 = UNCERTAINTY_MEASURE_WITH_UNIT (LENGTH_MEASURE( 1.000000000000000082E-05 ), #3892, 'distance_accuracy_value', 'NONE');
#16589 = DIRECTION ( 'NONE',  ( 0.000000000000000000, 0.000000000000000000, -1.000000000000000000 ) ) ;
#16590 = CARTESIAN_POINT ( 'NONE',  ( -22.99999999999999645, 68.00000000000000000, 37.00000000000002132 ) ) ;
#16591 = VECTOR ( 'NONE', #17820, 1000.000000000000000 ) ;
#16592 = ORIENTED_EDGE ( 'NONE', *, *, #9927, .F. ) ;
#16593 = ADVANCED_FACE ( 'NONE', ( #4232 ), #1399, .F. ) ;
#16594 = ORIENTED_EDGE ( 'NONE', *, *, #4148, .F. ) ;
#16595 = APPLICATION_CONTEXT ( 'automotive_design' ) ;
#16596 = EDGE_CURVE ( 'NONE', #8554, #6498, #17439, .T. ) ;
#16597 = SHAPE_REPRESENTATION ( 'Servo-Head', ( #2741 ), #14554 ) ;
#16598 = VERTEX_POINT ( 'NONE', #4627 ) ;
#16599 = VERTEX_POINT ( 'NONE', #12777 ) ;
#16600 = AXIS2_PLACEMENT_3D ( 'NONE', #6972, #19232, #8598 ) ;
#16601 = EDGE_CURVE ( 'NONE', #17763, #8286, #17394, .T. ) ;
#16602 = DIRECTION ( 'NONE',  ( 0.000000000000000000, 0.000000000000000000, 1.000000000000000000 ) ) ;
#16603 = DIRECTION ( 'NONE',  ( 1.000000000000000000, 0.000000000000000000, 0.000000000000000000 ) ) ;
#16604 = DIRECTION ( 'NONE',  ( 0.000000000000000000, 0.000000000000000000, 1.000000000000000000 ) ) ;
#16605 = SURFACE_SIDE_STYLE ('',( #6072 ) ) ;
#16606 = MECHANICAL_DESIGN_GEOMETRIC_PRESENTATION_REPRESENTATION (  '', ( #1204 ), #11640 ) ;
#16607 = AXIS2_PLACEMENT_3D ( 'NONE', #9313, #3444, #15819 ) ;
#16608 = DIRECTION ( 'NONE',  ( -0.000000000000000000, -1.000000000000000000, -0.000000000000000000 ) ) ;
#16609 =( NAMED_UNIT ( * ) PLANE_ANGLE_UNIT ( ) SI_UNIT ( $, .RADIAN. ) );
#16610 = AXIS2_PLACEMENT_3D ( 'NONE', #12178, #5693, #13733 ) ;
#16611 = DIRECTION ( 'NONE',  ( 0.000000000000000000, 0.000000000000000000, -1.000000000000000000 ) ) ;
#16612 = DIRECTION ( 'NONE',  ( -1.156482317317881191E-15, 0.000000000000000000, -1.000000000000000000 ) ) ;
#16613 = FACE_OUTER_BOUND ( 'NONE', #20001, .T. ) ;
#16614 = DIRECTION ( 'NONE',  ( -0.000000000000000000, -0.000000000000000000, 1.000000000000000000 ) ) ;
#16615 =( GEOMETRIC_REPRESENTATION_CONTEXT ( 3 ) GLOBAL_UNCERTAINTY_ASSIGNED_CONTEXT ( ( #13641 ) ) GLOBAL_UNIT_ASSIGNED_CONTEXT ( ( #6012, #18576, #4469 ) ) REPRESENTATION_CONTEXT ( 'NONE', 'WORKASPACE' ) );
#16616 = AXIS2_PLACEMENT_3D ( 'NONE', #4411, #18216, #6070 ) ;
#16617 = CARTESIAN_POINT ( 'NONE',  ( 31.00000000000003553, 10.00000000000000000, -23.00000000000000000 ) ) ;
#16618 = DIRECTION ( 'NONE',  ( -0.000000000000000000, -1.000000000000000000, -0.000000000000000000 ) ) ;
#16619 = FACE_OUTER_BOUND ( 'NONE', #4638, .T. ) ;
#16620 = VECTOR ( 'NONE', #14160, 1000.000000000000000 ) ;
#16621 = EDGE_CURVE ( 'NONE', #3581, #11558, #19023, .T. ) ;
#16622 = VERTEX_POINT ( 'NONE', #8027 ) ;
#16623 = AXIS2_PLACEMENT_3D ( 'NONE', #18759, #12396, #2995 ) ;
#16624 = ORIENTED_EDGE ( 'NONE', *, *, #17938, .T. ) ;
#16625 = VECTOR ( 'NONE', #10107, 1000.000000000000000 ) ;
#16626 = EDGE_LOOP ( 'NONE', ( #13372, #17435, #18979, #2142 ) ) ;
#16627 = EDGE_LOOP ( 'NONE', ( #15395, #5206, #14605, #10230 ) ) ;
#16628 = EDGE_CURVE ( 'NONE', #11436, #270, #14311, .T. ) ;
#16629 = COLOUR_RGB ( '', 0.09019608, 0.27058824, 0.51372549) ;
#16630 = CARTESIAN_POINT ( 'NONE',  ( -26.00000000000002842, 3.000000000000000000, 34.00000000000000711 ) ) ;
#16631 = CARTESIAN_POINT ( 'NONE',  ( 3.500000000000000000, -18.50000000000000000, -2.265596578422603396E-15 ) ) ;
#16632 = MECHANICAL_DESIGN_GEOMETRIC_PRESENTATION_REPRESENTATION (  '', ( #14640 ), #1440 ) ;
#16633 = FILL_AREA_STYLE ('',( #6941 ) ) ;
#16634 = AXIS2_PLACEMENT_3D ( 'NONE', #3737, #14658, #13129 ) ;
#16635 = CARTESIAN_POINT ( 'NONE',  ( -79.99999999999995737, 216.7545334744432921, 495.1946179577816451 ) ) ;
#16636 = LINE ( 'NONE', #1116, #2447 ) ;
#16637 = DIRECTION ( 'NONE',  ( -0.000000000000000000, -0.000000000000000000, 1.000000000000000000 ) ) ;
#16638 = VECTOR ( 'NONE', #10243, 1000.000000000000000 ) ;
#16639 = MECHANICAL_DESIGN_GEOMETRIC_PRESENTATION_REPRESENTATION (  '', ( #1448 ), #4122 ) ;
#16640 = STYLED_ITEM ( 'NONE', ( #14922 ), #15383 ) ;
#16641 = CARTESIAN_POINT ( 'NONE',  ( 35.99999999999999289, 6.000000000000000000, 21.99999999999999645 ) ) ;
#16642 = DIRECTION ( 'NONE',  ( 0.000000000000000000, -0.7699350945217658948, -0.6381222063396316813 ) ) ;
#16643 = DIRECTION ( 'NONE',  ( 0.000000000000000000, 1.000000000000000000, 0.000000000000000000 ) ) ;
#16644 = VECTOR ( 'NONE', #19107, 1000.000000000000000 ) ;
#16645 = ORIENTED_EDGE ( 'NONE', *, *, #15420, .T. ) ;
#16646 = DIRECTION ( 'NONE',  ( 1.000000000000000000, 9.815121534730717399E-17, 0.000000000000000000 ) ) ;
#16647 = DIRECTION ( 'NONE',  ( 1.000000000000000000, 5.889072920838430686E-16, -0.000000000000000000 ) ) ;
#16648 = VECTOR ( 'NONE', #10311, 1000.000000000000000 ) ;
#16649 = AXIS2_PLACEMENT_3D ( 'NONE', #16903, #2764, #17006 ) ;
#16650 = EDGE_CURVE ( 'NONE', #11661, #11725, #15680, .T. ) ;
#16651 = ORIENTED_EDGE ( 'NONE', *, *, #15034, .F. ) ;
#16652 = AXIS2_PLACEMENT_3D ( 'NONE', #15754, #4396, #3259 ) ;
#16653 = VECTOR ( 'NONE', #10648, 1000.000000000000000 ) ;
#16654 = ORIENTED_EDGE ( 'NONE', *, *, #549, .F. ) ;
#16655 = CARTESIAN_POINT ( 'NONE',  ( 53.48937290013659407, 145.9162550801369491, 0.000000000000000000 ) ) ;
#16656 = LINE ( 'NONE', #11897, #14481 ) ;
#16657 = VERTEX_POINT ( 'NONE', #7823 ) ;
#16658 = DIRECTION ( 'NONE',  ( 0.000000000000000000, 1.000000000000000000, 0.000000000000000000 ) ) ;
#16659 = CARTESIAN_POINT ( 'NONE',  ( -78.99999999999995737, 140.8764026050586722, 502.4686618848272133 ) ) ;
#16660 = CIRCLE ( 'NONE', #14345, 3.000000000000002665 ) ;
#16661 = CARTESIAN_POINT ( 'NONE',  ( -31.81980515339462912, 11.00000000000000000, -28.51980515339464972 ) ) ;
#16662 = CARTESIAN_POINT ( 'NONE',  ( 3.500000000000000000, 18.50000000000000000, 0.000000000000000000 ) ) ;
#16663 = LINE ( 'NONE', #4183, #12651 ) ;
#16664 = CYLINDRICAL_SURFACE ( 'NONE', #161, 3.000000000000000000 ) ;
#16665 = ORIENTED_EDGE ( 'NONE', *, *, #1672, .F. ) ;
#16666 = PLANE ( 'NONE',  #4893 ) ;
#16667 = DIRECTION ( 'NONE',  ( 0.000000000000000000, 1.000000000000000000, 0.000000000000000000 ) ) ;
#16668 =( NAMED_UNIT ( * ) PLANE_ANGLE_UNIT ( ) SI_UNIT ( $, .RADIAN. ) );
#16669 = DIRECTION ( 'NONE',  ( 1.000000000000000000, 5.889072920838430686E-16, -0.000000000000000000 ) ) ;
#16670 = ORIENTED_EDGE ( 'NONE', *, *, #7969, .T. ) ;
#16671 = ORIENTED_EDGE ( 'NONE', *, *, #7789, .T. ) ;
#16672 = STYLED_ITEM ( 'NONE', ( #12084 ), #2497 ) ;
#16673 = ORIENTED_EDGE ( 'NONE', *, *, #10869, .F. ) ;
#16674 = AXIS2_PLACEMENT_3D ( 'NONE', #6957, #5112, #13060 ) ;
#16675 = CARTESIAN_POINT ( 'NONE',  ( -40.00000000000000711, 10.00000000000000000, -26.00000000000000000 ) ) ;
#16676 = ADVANCED_FACE ( 'NONE', ( #12367 ), #17191, .F. ) ;
#16677 = ORIENTED_EDGE ( 'NONE', *, *, #16701, .F. ) ;
#16678 = LINE ( 'NONE', #13564, #15324 ) ;
#16679 = CARTESIAN_POINT ( 'NONE',  ( 0.000000000000000000, -3.000000000000000000, 0.000000000000000000 ) ) ;
#16680 = ORIENTED_EDGE ( 'NONE', *, *, #13574, .F. ) ;
#16681 = LINE ( 'NONE', #8919, #20230 ) ;
#16682 =( LENGTH_UNIT ( ) NAMED_UNIT ( * ) SI_UNIT ( .MILLI., .METRE. ) );
#16683 = DIRECTION ( 'NONE',  ( -0.000000000000000000, 1.000000000000000000, -0.000000000000000000 ) ) ;
#16684 = LINE ( 'NONE', #18493, #14881 ) ;
#16685 = AXIS2_PLACEMENT_3D ( 'NONE', #606, #514, #8355 ) ;
#16686 = CARTESIAN_POINT ( 'NONE',  ( -0.9999999956396431466, 139.1133280296707824, 488.5356365985891216 ) ) ;
#16687 = CYLINDRICAL_SURFACE ( 'NONE', #468, 3.883636366625808911 ) ;
#16688 = CYLINDRICAL_SURFACE ( 'NONE', #8171, 1.000000000000000888 ) ;
#16689 = EDGE_CURVE ( 'NONE', #7052, #6682, #1620, .T. ) ;
#16690 = CARTESIAN_POINT ( 'NONE',  ( 153.4893729001366864, 103.1299228374914492, 220.6387154965113382 ) ) ;
#16691 =( NAMED_UNIT ( * ) SI_UNIT ( $, .STERADIAN. ) SOLID_ANGLE_UNIT ( ) );
#16692 = AXIS2_PLACEMENT_3D ( 'NONE', #9149, #15446, #1275 ) ;
#16693 = SURFACE_STYLE_USAGE ( .BOTH. , #20038 ) ;
#16694 = DIRECTION ( 'NONE',  ( 0.000000000000000000, -1.000000000000000000, 0.000000000000000000 ) ) ;
#16695 = DIRECTION ( 'NONE',  ( 1.000000000000000000, 0.000000000000000000, 0.000000000000000000 ) ) ;
#16696 = CARTESIAN_POINT ( 'NONE',  ( 26.00000000000000355, 11.00000000000000000, -40.00000000000000711 ) ) ;
#16697 = ORIENTED_EDGE ( 'NONE', *, *, #13094, .T. ) ;
#16698 = CARTESIAN_POINT ( 'NONE',  ( 458.8334540492693350, 191.8198460455371333, 225.0057801310552463 ) ) ;
#16699 = ORIENTED_EDGE ( 'NONE', *, *, #7116, .T. ) ;
#16700 = UNCERTAINTY_MEASURE_WITH_UNIT (LENGTH_MEASURE( 1.000000000000000082E-05 ), #11287, 'distance_accuracy_value', 'NONE');
#16701 = EDGE_CURVE ( 'NONE', #11845, #504, #11209, .T. ) ;
#16702 = ORIENTED_EDGE ( 'NONE', *, *, #5878, .F. ) ;
#16703 = ADVANCED_FACE ( 'NONE', ( #17091 ), #6082, .F. ) ;
#16704 = ORIENTED_EDGE ( 'NONE', *, *, #6881, .T. ) ;
#16705 = FACE_OUTER_BOUND ( 'NONE', #14791, .T. ) ;
#16706 = DIRECTION ( 'NONE',  ( -1.000000000000000000, 0.000000000000000000, -0.000000000000000000 ) ) ;
#16707 = CARTESIAN_POINT ( 'NONE',  ( -30.99999999999999289, 68.00000000000000000, 31.00000000000000000 ) ) ;
#16708 = CYLINDRICAL_SURFACE ( 'NONE', #19176, 3.283624802691453848 ) ;
#16709 = EDGE_CURVE ( 'NONE', #4918, #6114, #6286, .T. ) ;
#16710 = CARTESIAN_POINT ( 'NONE',  ( -26.00000000000002842, 3.000000000000000000, -39.99999999999999289 ) ) ;
#16711 = DIRECTION ( 'NONE',  ( -0.000000000000000000, -0.000000000000000000, 1.000000000000000000 ) ) ;
#16712 = ADVANCED_FACE ( 'NONE', ( #12562 ), #18938, .F. ) ;
#16713 = DIRECTION ( 'NONE',  ( 1.000000000000000000, -0.000000000000000000, -0.000000000000000000 ) ) ;
#16714 = DIRECTION ( 'NONE',  ( 0.000000000000000000, 1.000000000000000000, 0.000000000000000000 ) ) ;
#16715 = EDGE_CURVE ( 'NONE', #18945, #8120, #946, .T. ) ;
#16716 = CARTESIAN_POINT ( 'NONE',  ( 20.99999999999996092, 3.000000000000000000, 32.50000000000000711 ) ) ;
#16717 = CARTESIAN_POINT ( 'NONE',  ( -37.00000000000000711, 10.00000000000000000, -18.00000000000000355 ) ) ;
#16718 =( NAMED_UNIT ( * ) SI_UNIT ( $, .STERADIAN. ) SOLID_ANGLE_UNIT ( ) );
#16719 = EDGE_CURVE ( 'NONE', #10815, #17493, #13195, .T. ) ;
#16720 = CARTESIAN_POINT ( 'NONE',  ( 5.941205806953520074, 0.000000000000000000, -15.14120580695351670 ) ) ;
#16721 = SHAPE_REPRESENTATION ( 'Part12^Assem2', ( #2741 ), #14604 ) ;
#16722 = ORIENTED_EDGE ( 'NONE', *, *, #7689, .T. ) ;
#16723 = ORIENTED_EDGE ( 'NONE', *, *, #11529, .F. ) ;
#16724 = EDGE_CURVE ( 'NONE', #17622, #2022, #652, .T. ) ;
#16725 = ORIENTED_EDGE ( 'NONE', *, *, #6239, .T. ) ;
#16726 = EDGE_LOOP ( 'NONE', ( #12195, #4027, #12488, #12829, #15944, #17113, #20045, #18766 ) ) ;
#16727 = LINE ( 'NONE', #11580, #16994 ) ;
#16728 =( NAMED_UNIT ( * ) PLANE_ANGLE_UNIT ( ) SI_UNIT ( $, .RADIAN. ) );
#16729 = UNCERTAINTY_MEASURE_WITH_UNIT (LENGTH_MEASURE( 1.000000000000000082E-05 ), #16168, 'distance_accuracy_value', 'NONE');
#16730 = CIRCLE ( 'NONE', #12094, 4.999999999999997335 ) ;
#16731 = CARTESIAN_POINT ( 'NONE',  ( -22.00000000000001776, 8.000000000000000000, 36.00000000000000711 ) ) ;
#16732 = SURFACE_STYLE_FILL_AREA ( #16633 ) ;
#16733 = LINE ( 'NONE', #14858, #13328 ) ;
#16734 =( NAMED_UNIT ( * ) PLANE_ANGLE_UNIT ( ) SI_UNIT ( $, .RADIAN. ) );
#16735 = EDGE_CURVE ( 'NONE', #345, #7788, #7265, .T. ) ;
#16736 = CARTESIAN_POINT ( 'NONE',  ( -35.00000000000000000, 19.00000000000000000, -21.00000000000000000 ) ) ;
#16737 = DIRECTION ( 'NONE',  ( 1.000000000000000000, 0.000000000000000000, 0.000000000000000000 ) ) ;
#16738 = CARTESIAN_POINT ( 'NONE',  ( -40.00000000000000711, 10.00000000000000000, 26.00000000000000000 ) ) ;
#16739 = CARTESIAN_POINT ( 'NONE',  ( 1.399999999999999911, 0.000000000000000000, 0.000000000000000000 ) ) ;
#16740 = ORIENTED_EDGE ( 'NONE', *, *, #4145, .T. ) ;
#16741 = DIRECTION ( 'NONE',  ( 0.000000000000000000, -1.000000000000000000, 0.000000000000000000 ) ) ;
#16742 = CARTESIAN_POINT ( 'NONE',  ( 0.000000000000000000, 0.000000000000000000, 0.000000000000000000 ) ) ;
#16743 = CARTESIAN_POINT ( 'NONE',  ( -211.5106270998635409, 123.1299228374912644, 170.4174721992565082 ) ) ;
#16744 = ADVANCED_FACE ( 'NONE', ( #7076, #13749, #7181, #10557, #12106, #7274 ), #13551, .T. ) ;
#16745 = ORIENTED_EDGE ( 'NONE', *, *, #5902, .T. ) ;
#16746 = AXIS2_PLACEMENT_3D ( 'NONE', #1284, #10600, #2963 ) ;
#16747 = ORIENTED_EDGE ( 'NONE', *, *, #1668, .F. ) ;
#16748 = UNCERTAINTY_MEASURE_WITH_UNIT (LENGTH_MEASURE( 1.000000000000000082E-05 ), #15242, 'distance_accuracy_value', 'NONE');
#16749 = ORIENTED_EDGE ( 'NONE', *, *, #12799, .T. ) ;
#16750 = CYLINDRICAL_SURFACE ( 'NONE', #137, 8.000000000000000000 ) ;
#16751 = LINE ( 'NONE', #4358, #10199 ) ;
#16752 = EDGE_LOOP ( 'NONE', ( #14064, #17426, #12470, #16677 ) ) ;
#16753 = CARTESIAN_POINT ( 'NONE',  ( 0.000000000000000000, 80.91625508013694912, -97.94896630388704750 ) ) ;
#16754 = DIRECTION ( 'NONE',  ( 0.000000000000000000, 0.000000000000000000, 1.000000000000000000 ) ) ;
#16755 = CIRCLE ( 'NONE', #592, 1.000000000000000888 ) ;
#16756 = LINE ( 'NONE', #13648, #6447 ) ;
#16757 = DIRECTION ( 'NONE',  ( 1.000000000000000000, 9.815121534730717399E-17, 0.000000000000000000 ) ) ;
#16758 = CARTESIAN_POINT ( 'NONE',  ( -75.00000000000000000, 313.8311070602663904, -142.2176018917206761 ) ) ;
#16759 = ORIENTED_EDGE ( 'NONE', *, *, #4532, .F. ) ;
#16760 = PRESENTATION_STYLE_ASSIGNMENT (( #18587 ) ) ;
#16761 = FACE_OUTER_BOUND ( 'NONE', #2314, .T. ) ;
#16762 = FILL_AREA_STYLE ('',( #756 ) ) ;
#16763 = APPLICATION_PROTOCOL_DEFINITION ( 'draft international standard', 'automotive_design', 1998, #9467 ) ;
#16764 = ORIENTED_EDGE ( 'NONE', *, *, #2223, .F. ) ;
#16765 = ORIENTED_EDGE ( 'NONE', *, *, #13292, .T. ) ;
#16766 = ORIENTED_EDGE ( 'NONE', *, *, #1221, .F. ) ;
#16767 = VERTEX_POINT ( 'NONE', #2519 ) ;
#16768 = PRESENTATION_LAYER_ASSIGNMENT (  '', '', ( #9165 ) ) ;
#16769 = ORIENTED_EDGE ( 'NONE', *, *, #13899, .T. ) ;
#16770 = DIRECTION ( 'NONE',  ( -0.000000000000000000, -1.000000000000000000, -0.000000000000000000 ) ) ;
#16771 = ORIENTED_EDGE ( 'NONE', *, *, #5718, .F. ) ;
#16772 = CARTESIAN_POINT ( 'NONE',  ( 25.99999999999999645, 11.00000000000000000, 40.00000000000000711 ) ) ;
#16773 = ORIENTED_EDGE ( 'NONE', *, *, #16715, .T. ) ;
#16774 = FILL_AREA_STYLE ('',( #19932 ) ) ;
#16775 = MECHANICAL_DESIGN_GEOMETRIC_PRESENTATION_REPRESENTATION (  '', ( #3936 ), #12494 ) ;
#16776 = ADVANCED_FACE ( 'NONE', ( #16454 ), #19916, .T. ) ;
#16777 = CIRCLE ( 'NONE', #16130, 3.299999999999997158 ) ;
#16778 = DIRECTION ( 'NONE',  ( -0.000000000000000000, -1.000000000000000000, -0.000000000000000000 ) ) ;
#16779 = DIRECTION ( 'NONE',  ( -0.000000000000000000, 1.000000000000000000, -0.000000000000000000 ) ) ;
#16780 = DIRECTION ( 'NONE',  ( -7.709882115452498874E-16, 0.000000000000000000, -1.000000000000000000 ) ) ;
#16781 = DIRECTION ( 'NONE',  ( 0.000000000000000000, -0.000000000000000000, -1.000000000000000000 ) ) ;
#16782 = SURFACE_STYLE_FILL_AREA ( #6168 ) ;
#16783 = CARTESIAN_POINT ( 'NONE',  ( 133.4893729001365728, 0.000000000000000000, 250.0000000000000000 ) ) ;
#16784 = ORIENTED_EDGE ( 'NONE', *, *, #14794, .F. ) ;
#16785 = ORIENTED_EDGE ( 'NONE', *, *, #19476, .T. ) ;
#16786 = AXIS2_PLACEMENT_3D ( 'NONE', #10673, #20024, #12324 ) ;
#16787 = VERTEX_POINT ( 'NONE', #7478 ) ;
#16788 = AXIS2_PLACEMENT_3D ( 'NONE', #3805, #10086, #2442 ) ;
#16789 = ORIENTED_EDGE ( 'NONE', *, *, #13753, .F. ) ;
#16790 = EDGE_CURVE ( 'NONE', #20243, #14026, #6610, .T. ) ;
#16791 = SURFACE_SIDE_STYLE ('',( #10799 ) ) ;
#16792 = CARTESIAN_POINT ( 'NONE',  ( -15.00000000000000000, 316.7545334744432353, 495.1946179577816451 ) ) ;
#16793 = DIRECTION ( 'NONE',  ( 1.000000000000000000, -6.123031769111888756E-17, 0.000000000000000000 ) ) ;
#16794 = SURFACE_STYLE_USAGE ( .BOTH. , #12356 ) ;
#16795 = DIRECTION ( 'NONE',  ( 1.000000000000000000, -0.000000000000000000, -0.000000000000000000 ) ) ;
#16796 = FACE_OUTER_BOUND ( 'NONE', #15154, .T. ) ;
#16797 = LINE ( 'NONE', #1282, #11354 ) ;
#16798 = PRESENTATION_STYLE_ASSIGNMENT (( #1190 ) ) ;
#16799 =( GEOMETRIC_REPRESENTATION_CONTEXT ( 3 ) GLOBAL_UNCERTAINTY_ASSIGNED_CONTEXT ( ( #19370 ) ) GLOBAL_UNIT_ASSIGNED_CONTEXT ( ( #1095, #1194, #7522 ) ) REPRESENTATION_CONTEXT ( 'NONE', 'WORKASPACE' ) );
#16800 = CYLINDRICAL_SURFACE ( 'NONE', #2066, 3.000000000000002665 ) ;
#16801 = DIRECTION ( 'NONE',  ( 0.000000000000000000, 0.000000000000000000, 1.000000000000000000 ) ) ;
#16802 = CIRCLE ( 'NONE', #16786, 3.000000000000002665 ) ;
#16803 = EDGE_CURVE ( 'NONE', #3885, #19179, #10247, .T. ) ;
#16804 = CIRCLE ( 'NONE', #1625, 17.85000000000000142 ) ;
#16805 = DIRECTION ( 'NONE',  ( -0.000000000000000000, -1.000000000000000000, 0.000000000000000000 ) ) ;
#16806 = DIRECTION ( 'NONE',  ( 5.551115123125777022E-14, 0.000000000000000000, -1.000000000000000000 ) ) ;
#16807 = EDGE_CURVE ( 'NONE', #3908, #1145, #8596, .T. ) ;
#16808 = EDGE_LOOP ( 'NONE', ( #13720, #16759, #3706, #17734, #10938, #235 ) ) ;
#16809 = ORIENTED_EDGE ( 'NONE', *, *, #18808, .F. ) ;
#16810 = VERTEX_POINT ( 'NONE', #2409 ) ;
#16811 =( NAMED_UNIT ( * ) SI_UNIT ( $, .STERADIAN. ) SOLID_ANGLE_UNIT ( ) );
#16812 = ORIENTED_EDGE ( 'NONE', *, *, #1914, .F. ) ;
#16813 = ORIENTED_EDGE ( 'NONE', *, *, #662, .T. ) ;
#16814 = DIRECTION ( 'NONE',  ( 0.000000000000000000, 1.000000000000000000, 0.000000000000000000 ) ) ;
#16815 =( GEOMETRIC_REPRESENTATION_CONTEXT ( 3 ) GLOBAL_UNCERTAINTY_ASSIGNED_CONTEXT ( ( #7035 ) ) GLOBAL_UNIT_ASSIGNED_CONTEXT ( ( #18526, #4015, #13710 ) ) REPRESENTATION_CONTEXT ( 'NONE', 'WORKASPACE' ) );
#16816 = EDGE_CURVE ( 'NONE', #4851, #19516, #15836, .T. ) ;
#16817 = PRESENTATION_LAYER_ASSIGNMENT (  '', '', ( #11542 ) ) ;
#16818 = VECTOR ( 'NONE', #11984, 1000.000000000000000 ) ;
#16819 = DIRECTION ( 'NONE',  ( -0.000000000000000000, -0.000000000000000000, 1.000000000000000000 ) ) ;
#16820 = DIRECTION ( 'NONE',  ( -1.000000000000000000, 0.000000000000000000, -0.000000000000000000 ) ) ;
#16821 = EDGE_CURVE ( 'NONE', #13927, #14143, #15099, .T. ) ;
#16822 = CARTESIAN_POINT ( 'NONE',  ( 0.000000000000000000, 0.000000000000000000, 250.0000000000000000 ) ) ;
#16823 = DIRECTION ( 'NONE',  ( -0.000000000000000000, -1.000000000000000000, -0.000000000000000000 ) ) ;
#16824 = DIRECTION ( 'NONE',  ( 1.000000000000000000, 5.889072920838430686E-16, -0.000000000000000000 ) ) ;
#16825 = CARTESIAN_POINT ( 'NONE',  ( 31.00000000000006750, 19.00000000000000000, -21.00000000000000355 ) ) ;
#16826 = CARTESIAN_POINT ( 'NONE',  ( -26.00000000000000000, 19.00000000000000000, -31.00000000000003908 ) ) ;
#16827 = DIRECTION ( 'NONE',  ( 0.000000000000000000, 0.000000000000000000, -1.000000000000000000 ) ) ;
#16828 = DIRECTION ( 'NONE',  ( 1.000000000000000000, 2.135044278125300850E-16, -0.000000000000000000 ) ) ;
#16829 = CARTESIAN_POINT ( 'NONE',  ( -80.49355071749218382, 139.7917123817078959, 489.4303101983043689 ) ) ;
#16830 = CARTESIAN_POINT ( 'NONE',  ( -18.00000000000001421, 6.000000000000000000, 40.00000000000000711 ) ) ;
#16831 = ADVANCED_FACE ( 'NONE', ( #16761 ), #12197, .F. ) ;
#16832 = ORIENTED_EDGE ( 'NONE', *, *, #2858, .F. ) ;
#16833 = VECTOR ( 'NONE', #11473, 1000.000000000000000 ) ;
#16834 = EDGE_CURVE ( 'NONE', #2874, #19410, #20234, .T. ) ;
#16835 = ORIENTED_EDGE ( 'NONE', *, *, #14982, .F. ) ;
#16836 = ADVANCED_FACE ( 'NONE', ( #12299 ), #4574, .T. ) ;
#16837 = ORIENTED_EDGE ( 'NONE', *, *, #17555, .F. ) ;
#16838 = CARTESIAN_POINT ( 'NONE',  ( 22.99999999999995737, 3.000000000000000000, -33.99999999999998579 ) ) ;
#16839 = AXIS2_PLACEMENT_3D ( 'NONE', #19536, #13192, #13400 ) ;
#16840 = DIRECTION ( 'NONE',  ( 0.000000000000000000, 1.000000000000000000, 0.000000000000000000 ) ) ;
#16841 = VERTEX_POINT ( 'NONE', #15407 ) ;
#16842 = CARTESIAN_POINT ( 'NONE',  ( -33.00000000000000000, 10.00000000000000000, -26.00000000000000355 ) ) ;
#16843 = SURFACE_SIDE_STYLE ('',( #12100 ) ) ;
#16844 = FILL_AREA_STYLE ('',( #18366 ) ) ;
#16845 = AXIS2_PLACEMENT_3D ( 'NONE', #15761, #9351, #6177 ) ;
#16846 = CARTESIAN_POINT ( 'NONE',  ( -80.01145065471625628, 141.3451996134640751, 501.6408122255736544 ) ) ;
#16847 = FACE_OUTER_BOUND ( 'NONE', #4029, .T. ) ;
#16848 = SURFACE_SIDE_STYLE ('',( #4364 ) ) ;
#16849 = ORIENTED_EDGE ( 'NONE', *, *, #16719, .F. ) ;
#16850 = APPLICATION_CONTEXT ( 'automotive_design' ) ;
#16851 = SURFACE_STYLE_FILL_AREA ( #4074 ) ;
#16852 = DIRECTION ( 'NONE',  ( 1.000000000000000000, 9.815121534730717399E-17, 0.000000000000000000 ) ) ;
#16853 = PRODUCT_CONTEXT ( 'NONE', #14462, 'mechanical' ) ;
#16854 = ORIENTED_EDGE ( 'NONE', *, *, #8169, .T. ) ;
#16855 = CARTESIAN_POINT ( 'NONE',  ( -26.00000000000000000, 11.00000000000000000, -40.00000000000000711 ) ) ;
#16856 = ADVANCED_FACE ( 'NONE', ( #6232 ), #20328, .T. ) ;
#16857 = ORIENTED_EDGE ( 'NONE', *, *, #10264, .F. ) ;
#16858 = AXIS2_PLACEMENT_3D ( 'NONE', #10994, #6570, #1690 ) ;
#16859 = ORIENTED_EDGE ( 'NONE', *, *, #17222, .T. ) ;
#16860 = ORIENTED_EDGE ( 'NONE', *, *, #17192, .F. ) ;
#16861 = ADVANCED_FACE ( 'NONE', ( #13847 ), #9310, .T. ) ;
#16862 = LINE ( 'NONE', #7384, #18607 ) ;
#16863 = VECTOR ( 'NONE', #12981, 1000.000000000000000 ) ;
#16864 = ORIENTED_EDGE ( 'NONE', *, *, #9530, .F. ) ;
#16865 = CYLINDRICAL_SURFACE ( 'NONE', #8062, 5.000000000000000888 ) ;
#16866 = CARTESIAN_POINT ( 'NONE',  ( 0.6600482361318578128, 140.4535475171542771, 500.8793675648332169 ) ) ;
#16867 = VERTEX_POINT ( 'NONE', #7567 ) ;
#16868 =( NAMED_UNIT ( * ) PLANE_ANGLE_UNIT ( ) SI_UNIT ( $, .RADIAN. ) );
#16869 = CARTESIAN_POINT ( 'NONE',  ( 153.4893729001366864, 103.1299228374914492, 220.6387154965113382 ) ) ;
#16870 = DIRECTION ( 'NONE',  ( 6.123031769111888756E-17, 0.000000000000000000, 1.000000000000000000 ) ) ;
#16871 = VECTOR ( 'NONE', #6591, 1000.000000000000000 ) ;
#16872 = MECHANICAL_DESIGN_GEOMETRIC_PRESENTATION_REPRESENTATION (  '', ( #9279 ), #12253 ) ;
#16873 = FACE_OUTER_BOUND ( 'NONE', #4494, .T. ) ;
#16874 = CARTESIAN_POINT ( 'NONE',  ( 498.8334540492693918, 167.8734308960555950, 250.0000000000000000 ) ) ;
#16875 = CARTESIAN_POINT ( 'NONE',  ( 5.950000000000000178, 0.000000000000000000, 0.000000000000000000 ) ) ;
#16876 = AXIS2_PLACEMENT_3D ( 'NONE', #19251, #8516, #3588 ) ;
#16877 = LINE ( 'NONE', #2742, #1219 ) ;
#16878 = SURFACE_STYLE_FILL_AREA ( #8836 ) ;
#16879 = DIRECTION ( 'NONE',  ( 1.000000000000000000, -0.000000000000000000, -0.000000000000000000 ) ) ;
#16880 = CARTESIAN_POINT ( 'NONE',  ( 0.000000000000000000, 0.000000000000000000, 0.000000000000000000 ) ) ;
#16881 = PRODUCT_DEFINITION_FORMATION_WITH_SPECIFIED_SOURCE ( 'ANY', '', #208, .NOT_KNOWN. ) ;
#16882 = CIRCLE ( 'NONE', #3027, 2.999999999999995559 ) ;
#16883 = LINE ( 'NONE', #4211, #3003 ) ;
#16884 = VECTOR ( 'NONE', #10942, 1000.000000000000000 ) ;
#16885 = DIRECTION ( 'NONE',  ( -1.000000000000000000, -0.000000000000000000, -0.000000000000000000 ) ) ;
#16886 = ORIENTED_EDGE ( 'NONE', *, *, #2045, .T. ) ;
#16887 = EDGE_LOOP ( 'NONE', ( #19597, #2422 ) ) ;
#16888 = VECTOR ( 'NONE', #15163, 1000.000000000000000 ) ;
#16889 = STYLED_ITEM ( 'NONE', ( #9486 ), #18329 ) ;
#16890 = ORIENTED_EDGE ( 'NONE', *, *, #4561, .F. ) ;
#16891 = ADVANCED_FACE ( 'NONE', ( #7868 ), #18780, .T. ) ;
#16892 = VECTOR ( 'NONE', #5121, 1000.000000000000000 ) ;
#16893 = ORIENTED_EDGE ( 'NONE', *, *, #18890, .F. ) ;
#16894 = FACE_OUTER_BOUND ( 'NONE', #9163, .T. ) ;
#16895 = VERTEX_POINT ( 'NONE', #1337 ) ;
#16896 = CARTESIAN_POINT ( 'NONE',  ( 3.000000000000000000, 41.00000000000000711, 6.000000000000000000 ) ) ;
#16897 = SURFACE_STYLE_FILL_AREA ( #8940 ) ;
#16898 = DIRECTION ( 'NONE',  ( -0.000000000000000000, -1.000000000000000000, -0.000000000000000000 ) ) ;
#16899 = PRESENTATION_LAYER_ASSIGNMENT (  '', '', ( #1204 ) ) ;
#16900 = ORIENTED_EDGE ( 'NONE', *, *, #14519, .T. ) ;
#16901 = LINE ( 'NONE', #6279, #13799 ) ;
#16902 = CYLINDRICAL_SURFACE ( 'NONE', #1838, 10.00000000000000888 ) ;
#16903 = CARTESIAN_POINT ( 'NONE',  ( 498.8334540492693918, 191.8198460455371333, 225.0057801310552463 ) ) ;
#16904 = DIRECTION ( 'NONE',  ( -1.000000000000000000, -0.000000000000000000, -0.000000000000000000 ) ) ;
#16905 = FILL_AREA_STYLE_COLOUR ( '', #14194 ) ;
#16906 = EDGE_CURVE ( 'NONE', #6446, #258, #9714, .T. ) ;
#16907 = AXIS2_PLACEMENT_3D ( 'NONE', #5173, #11445, #17723 ) ;
#16908 = MECHANICAL_DESIGN_GEOMETRIC_PRESENTATION_REPRESENTATION (  '', ( #4391 ), #17533 ) ;
#16909 = ORIENTED_EDGE ( 'NONE', *, *, #6243, .T. ) ;
#16910 = VERTEX_POINT ( 'NONE', #12418 ) ;
#16911 = EDGE_LOOP ( 'NONE', ( #3730, #12346, #6270, #8292 ) ) ;
#16912 = DIRECTION ( 'NONE',  ( -1.000000000000000000, -9.815121534730717399E-17, 0.000000000000000000 ) ) ;
#16913 = ORIENTED_EDGE ( 'NONE', *, *, #187, .T. ) ;
#16914 = ORIENTED_EDGE ( 'NONE', *, *, #7451, .F. ) ;
#16915 = AXIS2_PLACEMENT_3D ( 'NONE', #18589, #10558, #9005 ) ;
#16916 = CARTESIAN_POINT ( 'NONE',  ( 0.000000000000000000, 3.000000000000000000, -36.50000000000000000 ) ) ;
#16917 = CARTESIAN_POINT ( 'NONE',  ( 53.48937290013660828, 34.32473510485366575, 0.000000000000000000 ) ) ;
#16918 = UNCERTAINTY_MEASURE_WITH_UNIT (LENGTH_MEASURE( 1.000000000000000082E-05 ), #3480, 'distance_accuracy_value', 'NONE');
#16919 = EDGE_CURVE ( 'NONE', #6379, #13294, #3977, .T. ) ;
#16920 = DIRECTION ( 'NONE',  ( 1.000000000000000000, -0.000000000000000000, -0.000000000000000000 ) ) ;
#16921 = CARTESIAN_POINT ( 'NONE',  ( 5.162501635565829972, 0.000000000000000000, 0.000000000000000000 ) ) ;
#16922 = MECHANICAL_DESIGN_GEOMETRIC_PRESENTATION_REPRESENTATION (  '', ( #15269 ), #1097 ) ;
#16923 = MECHANICAL_DESIGN_GEOMETRIC_PRESENTATION_REPRESENTATION (  '', ( #9643 ), #3416 ) ;
#16924 = PRODUCT_RELATED_PRODUCT_CATEGORY ( 'part', '', ( #17662 ) ) ;
#16925 = CARTESIAN_POINT ( 'NONE',  ( -41.50085094405408626, 193.0431417881923153, 510.3921618609452935 ) ) ;
#16926 = DIRECTION ( 'NONE',  ( -0.000000000000000000, 0.000000000000000000, 1.000000000000000000 ) ) ;
#16927 = PLANE ( 'NONE',  #4361 ) ;
#16928 = DIRECTION ( 'NONE',  ( -0.000000000000000000, -0.000000000000000000, 1.000000000000000000 ) ) ;
#16929 = ORIENTED_EDGE ( 'NONE', *, *, #11025, .T. ) ;
#16930 = FACE_OUTER_BOUND ( 'NONE', #13747, .T. ) ;
#16931 = PLANE ( 'NONE',  #3768 ) ;
#16932 = ADVANCED_FACE ( 'NONE', ( #11070 ), #1656, .F. ) ;
#16933 = PRESENTATION_LAYER_ASSIGNMENT (  '', '', ( #13630 ) ) ;
#16934 = EDGE_CURVE ( 'NONE', #9586, #6469, #20119, .T. ) ;
#16935 = VECTOR ( 'NONE', #5389, 1000.000000000000000 ) ;
#16936 = CIRCLE ( 'NONE', #19227, 5.000000000000000888 ) ;
#16937 = ORIENTED_EDGE ( 'NONE', *, *, #5552, .T. ) ;
#16938 = AXIS2_PLACEMENT_3D ( 'NONE', #12918, #17644, #19180 ) ;
#16939 = ADVANCED_FACE ( 'NONE', ( #19392 ), #19752, .F. ) ;
#16940 = ORIENTED_EDGE ( 'NONE', *, *, #10636, .F. ) ;
#16941 = VECTOR ( 'NONE', #3013, 1000.000000000000000 ) ;
#16942 = PRESENTATION_LAYER_ASSIGNMENT (  '', '', ( #14301 ) ) ;
#16943 = DIRECTION ( 'NONE',  ( 0.000000000000000000, 0.000000000000000000, 1.000000000000000000 ) ) ;
#16944 =( GEOMETRIC_REPRESENTATION_CONTEXT ( 3 ) GLOBAL_UNCERTAINTY_ASSIGNED_CONTEXT ( ( #11561 ) ) GLOBAL_UNIT_ASSIGNED_CONTEXT ( ( #6209, #1531, #11134 ) ) REPRESENTATION_CONTEXT ( 'NONE', 'WORKASPACE' ) );
#16945 = ORIENTED_EDGE ( 'NONE', *, *, #16444, .T. ) ;
#16946 = CARTESIAN_POINT ( 'NONE',  ( -36.99999999999997868, 3.000000000000000000, -22.99999999999999645 ) ) ;
#16947 = DIRECTION ( 'NONE',  ( 1.000000000000000000, 0.000000000000000000, 0.000000000000000000 ) ) ;
#16948 = CIRCLE ( 'NONE', #10688, 10.00000000000000888 ) ;
#16949 = EDGE_CURVE ( 'NONE', #17127, #11075, #985, .T. ) ;
#16950 = CARTESIAN_POINT ( 'NONE',  ( 111.4893729001366154, 77.72476844875745883, 252.0000000000000000 ) ) ;
#16951 = EDGE_CURVE ( 'NONE', #14513, #12416, #5097, .T. ) ;
#16952 = CARTESIAN_POINT ( 'NONE',  ( -75.00000000000000000, 313.8311070602663904, -142.2176018917206761 ) ) ;
#16953 = PLANE ( 'NONE',  #11345 ) ;
#16954 = ORIENTED_EDGE ( 'NONE', *, *, #10288, .F. ) ;
#16955 = DIRECTION ( 'NONE',  ( 0.000000000000000000, 1.000000000000000000, 0.000000000000000000 ) ) ;
#16956 = ORIENTED_EDGE ( 'NONE', *, *, #7759, .T. ) ;
#16957 = CARTESIAN_POINT ( 'NONE',  ( 0.000000000000000000, 0.000000000000000000, 515.1946179577817020 ) ) ;
#16958 = DIRECTION ( 'NONE',  ( 0.000000000000000000, -1.000000000000000000, 0.000000000000000000 ) ) ;
#16959 = PRODUCT_CONTEXT ( 'NONE', #8815, 'mechanical' ) ;
#16960 = EDGE_CURVE ( 'NONE', #11944, #11746, #1871, .T. ) ;
#16961 = ORIENTED_EDGE ( 'NONE', *, *, #20251, .T. ) ;
#16962 = ORIENTED_EDGE ( 'NONE', *, *, #6494, .F. ) ;
#16963 = PRESENTATION_STYLE_ASSIGNMENT (( #16558 ) ) ;
#16964 = EDGE_CURVE ( 'NONE', #16331, #4741, #13838, .T. ) ;
#16965 = ORIENTED_EDGE ( 'NONE', *, *, #17062, .T. ) ;
#16966 = AXIS2_PLACEMENT_3D ( 'NONE', #1032, #13647, #13944 ) ;
#16967 = ORIENTED_EDGE ( 'NONE', *, *, #14433, .T. ) ;
#16968 = CONICAL_SURFACE ( 'NONE', #8074, 18.17500000000000071, 0.7483780475235185525 ) ;
#16969 = VERTEX_POINT ( 'NONE', #14458 ) ;
#16970 = CIRCLE ( 'NONE', #15340, 1.000000000000000888 ) ;
#16971 = FACE_OUTER_BOUND ( 'NONE', #13223, .T. ) ;
#16972 = ORIENTED_EDGE ( 'NONE', *, *, #16344, .T. ) ;
#16973 = FACE_OUTER_BOUND ( 'NONE', #19716, .T. ) ;
#16974 = VECTOR ( 'NONE', #9430, 1000.000000000000000 ) ;
#16975 = CARTESIAN_POINT ( 'NONE',  ( 31.99999999999998579, 10.00000000000000000, 22.99999999999999645 ) ) ;
#16976 = CARTESIAN_POINT ( 'NONE',  ( 486.8117674897343363, 134.2156642432025251, 250.0000000000000000 ) ) ;
#16977 = FACE_OUTER_BOUND ( 'NONE', #16293, .T. ) ;
#16978 = DIRECTION ( 'NONE',  ( 0.000000000000000000, 0.000000000000000000, 1.000000000000000000 ) ) ;
#16979 = DIRECTION ( 'NONE',  ( 0.000000000000000000, 0.000000000000000000, -1.000000000000000000 ) ) ;
#16980 =( LENGTH_UNIT ( ) NAMED_UNIT ( * ) SI_UNIT ( .MILLI., .METRE. ) );
#16981 =( NAMED_UNIT ( * ) PLANE_ANGLE_UNIT ( ) SI_UNIT ( $, .RADIAN. ) );
#16982 = DIRECTION ( 'NONE',  ( 1.000000000000000000, -0.000000000000000000, -0.000000000000000000 ) ) ;
#16983 = EDGE_CURVE ( 'NONE', #8866, #14996, #15924, .T. ) ;
#16984 = DIRECTION ( 'NONE',  ( 0.000000000000000000, 0.000000000000000000, 1.000000000000000000 ) ) ;
#16985 = CARTESIAN_POINT ( 'NONE',  ( 25.99999999999996092, 0.000000000000000000, -31.00000000000003197 ) ) ;
#16986 = CARTESIAN_POINT ( 'NONE',  ( 30.90550859392669025, 32.88608451763353457, 66.87703344121200644 ) ) ;
#16987 = CARTESIAN_POINT ( 'NONE',  ( 3.850000000000000089, 0.000000000000000000, -14.27500000000000036 ) ) ;
#16988 = PLANE ( 'NONE',  #9291 ) ;
#16989 = PRESENTATION_LAYER_ASSIGNMENT (  '', '', ( #16672 ) ) ;
#16990 = ADVANCED_FACE ( 'NONE', ( #18118 ), #9930, .T. ) ;
#16991 = CARTESIAN_POINT ( 'NONE',  ( -39.99999999999997868, 3.000000000000000000, -25.99999999999999645 ) ) ;
#16992 = ORIENTED_EDGE ( 'NONE', *, *, #18547, .F. ) ;
#16993 = EDGE_CURVE ( 'NONE', #18959, #36, #8771, .T. ) ;
#16994 = VECTOR ( 'NONE', #13241, 1000.000000000000000 ) ;
#16995 = ORIENTED_EDGE ( 'NONE', *, *, #4514, .T. ) ;
#16996 = PRODUCT_DEFINITION_SHAPE ( 'NONE', 'NONE',  #20383 ) ;
#16997 = ORIENTED_EDGE ( 'NONE', *, *, #8756, .F. ) ;
#16998 = FACE_OUTER_BOUND ( 'NONE', #1493, .T. ) ;
#16999 = ORIENTED_EDGE ( 'NONE', *, *, #385, .F. ) ;
#17000 = VECTOR ( 'NONE', #15160, 1000.000000000000227 ) ;
#17001 = FACE_OUTER_BOUND ( 'NONE', #12903, .T. ) ;
#17002 =( LENGTH_UNIT ( ) NAMED_UNIT ( * ) SI_UNIT ( .MILLI., .METRE. ) );
#17003 = EDGE_LOOP ( 'NONE', ( #15715, #19287 ) ) ;
#17004 = FILL_AREA_STYLE ('',( #4524 ) ) ;
#17005 = LINE ( 'NONE', #18638, #19598 ) ;
#17006 = DIRECTION ( 'NONE',  ( 0.000000000000000000, 0.000000000000000000, -1.000000000000000000 ) ) ;
#17007 =( LENGTH_UNIT ( ) NAMED_UNIT ( * ) SI_UNIT ( .MILLI., .METRE. ) );
#17008 = FACE_OUTER_BOUND ( 'NONE', #9592, .T. ) ;
#17009 = PLANE ( 'NONE',  #18123 ) ;
#17010 = EDGE_CURVE ( 'NONE', #19977, #13760, #5202, .T. ) ;
#17011 = SURFACE_STYLE_USAGE ( .BOTH. , #15365 ) ;
#17012 = LINE ( 'NONE', #7435, #17260 ) ;
#17013 = ORIENTED_EDGE ( 'NONE', *, *, #446, .T. ) ;
#17014 = VECTOR ( 'NONE', #11724, 1000.000000000000000 ) ;
#17015 = ORIENTED_EDGE ( 'NONE', *, *, #20174, .T. ) ;
#17016 = ORIENTED_EDGE ( 'NONE', *, *, #7006, .F. ) ;
#17017 = CARTESIAN_POINT ( 'NONE',  ( 0.000000000000000000, 317.7545334744432353, 1.632680918566406547E-16 ) ) ;
#17018 = EDGE_LOOP ( 'NONE', ( #5766, #7574, #3880, #5532 ) ) ;
#17019 = VERTEX_POINT ( 'NONE', #6856 ) ;
#17020 = ORIENTED_EDGE ( 'NONE', *, *, #4348, .F. ) ;
#17021 = LINE ( 'NONE', #4542, #525 ) ;
#17022 = FILL_AREA_STYLE_COLOUR ( '', #7691 ) ;
#17023 = CYLINDRICAL_SURFACE ( 'NONE', #996, 3.000000000000002665 ) ;
#17024 = DIRECTION ( 'NONE',  ( 0.000000000000000000, 0.000000000000000000, -1.000000000000000000 ) ) ;
#17025 =( LENGTH_UNIT ( ) NAMED_UNIT ( * ) SI_UNIT ( .MILLI., .METRE. ) );
#17026 = DIRECTION ( 'NONE',  ( -1.000000000000000000, -0.000000000000000000, 3.854941057726258312E-16 ) ) ;
#17027 = CARTESIAN_POINT ( 'NONE',  ( 53.48937290013659407, 129.7247684487574304, 281.6050404526570219 ) ) ;
#17028 = DIRECTION ( 'NONE',  ( -0.000000000000000000, -1.000000000000000000, -0.000000000000000000 ) ) ;
#17029 =( NAMED_UNIT ( * ) SI_UNIT ( $, .STERADIAN. ) SOLID_ANGLE_UNIT ( ) );
#17030 = VERTEX_POINT ( 'NONE', #10304 ) ;
#17031 = DIRECTION ( 'NONE',  ( 0.000000000000000000, 0.000000000000000000, -1.000000000000000000 ) ) ;
#17032 = DIRECTION ( 'NONE',  ( -0.000000000000000000, 1.000000000000000000, -0.000000000000000000 ) ) ;
#17033 = DIRECTION ( 'NONE',  ( 0.000000000000000000, 0.000000000000000000, 1.000000000000000000 ) ) ;
#17034 = MECHANICAL_DESIGN_GEOMETRIC_PRESENTATION_REPRESENTATION (  '', ( #5517 ), #9799 ) ;
#17035 = ORIENTED_EDGE ( 'NONE', *, *, #15711, .F. ) ;
#17036 = CARTESIAN_POINT ( 'NONE',  ( -211.5106270998635409, 123.1299228374912644, 220.6387154965113382 ) ) ;
#17037 = ORIENTED_EDGE ( 'NONE', *, *, #2427, .F. ) ;
#17038 = EDGE_CURVE ( 'NONE', #16787, #11555, #8189, .T. ) ;
#17039 = DIRECTION ( 'NONE',  ( 1.000000000000000000, -0.000000000000000000, 0.000000000000000000 ) ) ;
#17040 = VERTEX_POINT ( 'NONE', #13049 ) ;
#17041 = CARTESIAN_POINT ( 'NONE',  ( -41.50085094405408626, 209.4098724938429541, 510.3921618609452935 ) ) ;
#17042 = DIRECTION ( 'NONE',  ( -0.000000000000000000, -1.000000000000000000, 0.000000000000000000 ) ) ;
#17043 = CONICAL_SURFACE ( 'NONE', #12775, 1.800000000000000266, 0.7853981633974524978 ) ;
#17044 = CARTESIAN_POINT ( 'NONE',  ( 35.99999999999999289, 6.000000000000000000, 21.99999999999999645 ) ) ;
#17045 = CARTESIAN_POINT ( 'NONE',  ( -77.99033078109006567, 49.66333933884486385, 252.0000000000000000 ) ) ;
#17046 = DIRECTION ( 'NONE',  ( -0.000000000000000000, -0.000000000000000000, 1.000000000000000000 ) ) ;
#17047 = VECTOR ( 'NONE', #493, 1000.000000000000000 ) ;
#17048 = VERTEX_POINT ( 'NONE', #334 ) ;
#17049 = DIRECTION ( 'NONE',  ( -0.000000000000000000, 1.000000000000000000, -0.000000000000000000 ) ) ;
#17050 = CARTESIAN_POINT ( 'NONE',  ( 0.000000000000000000, 316.7545334744432353, 515.1946179577817020 ) ) ;
#17051 = EDGE_CURVE ( 'NONE', #5279, #9984, #11160, .T. ) ;
#17052 = VERTEX_POINT ( 'NONE', #12826 ) ;
#17053 = EDGE_LOOP ( 'NONE', ( #17399, #17371, #18744, #15232 ) ) ;
#17054 = ORIENTED_EDGE ( 'NONE', *, *, #14015, .F. ) ;
#17055 = EDGE_CURVE ( 'NONE', #16024, #13405, #9728, .T. ) ;
#17056 = EDGE_LOOP ( 'NONE', ( #17200, #18155, #19200, #1974 ) ) ;
#17057 = EDGE_CURVE ( 'NONE', #14021, #6358, #1966, .T. ) ;
#17058 = CARTESIAN_POINT ( 'NONE',  ( 133.4893729001365443, 113.1299228374914634, 79.58252780074349175 ) ) ;
#17059 = VECTOR ( 'NONE', #18615, 1000.000000000000000 ) ;
#17060 = VERTEX_POINT ( 'NONE', #17437 ) ;
#17061 = CARTESIAN_POINT ( 'NONE',  ( -38.50085094405407204, 209.4098724938429541, 510.3921618609452935 ) ) ;
#17062 = EDGE_CURVE ( 'NONE', #9818, #17052, #19195, .T. ) ;
#17063 = CARTESIAN_POINT ( 'NONE',  ( 423.8334540492694487, 191.8198460455371333, 34.99421986894476788 ) ) ;
#17064 = CARTESIAN_POINT ( 'NONE',  ( -79.99999999999995737, 219.7545334744433205, 515.1946179577817020 ) ) ;
#17065 = ADVANCED_FACE ( 'NONE', ( #17543 ), #11375, .F. ) ;
#17066 = CARTESIAN_POINT ( 'NONE',  ( -79.99999999999995737, 142.0976792249508946, 502.3210940490797611 ) ) ;
#17067 = CARTESIAN_POINT ( 'NONE',  ( 498.8334540492693918, 191.8198460455371333, 168.2339398819845826 ) ) ;
#17068 = CARTESIAN_POINT ( 'NONE',  ( 178.4893729001365443, 145.9162550801369491, 0.000000000000000000 ) ) ;
#17069 =( NAMED_UNIT ( * ) SI_UNIT ( $, .STERADIAN. ) SOLID_ANGLE_UNIT ( ) );
#17070 = CARTESIAN_POINT ( 'NONE',  ( -23.00000000000002487, 0.000000000000000000, -36.99999999999999289 ) ) ;
#17071 = LINE ( 'NONE', #9031, #18681 ) ;
#17072 = DIRECTION ( 'NONE',  ( 0.000000000000000000, 0.000000000000000000, -1.000000000000000000 ) ) ;
#17073 = CARTESIAN_POINT ( 'NONE',  ( 0.000000000000000000, 0.000000000000000000, 0.000000000000000000 ) ) ;
#17074 = PLANE ( 'NONE',  #12495 ) ;
#17075 = EDGE_CURVE ( 'NONE', #17453, #4266, #17659, .T. ) ;
#17076 = CARTESIAN_POINT ( 'NONE',  ( 78.48937290013660117, 103.1299228374914065, 29.36128450348865471 ) ) ;
#17077 = EDGE_CURVE ( 'NONE', #15076, #19612, #14184, .T. ) ;
#17078 = ORIENTED_EDGE ( 'NONE', *, *, #7049, .F. ) ;
#17079 = ORIENTED_EDGE ( 'NONE', *, *, #655, .F. ) ;
#17080 = EDGE_CURVE ( 'NONE', #1902, #6860, #18332, .T. ) ;
#17081 = PRESENTATION_LAYER_ASSIGNMENT (  '', '', ( #3965 ) ) ;
#17082 = DIRECTION ( 'NONE',  ( 1.000000000000000000, 0.000000000000000000, 0.000000000000000000 ) ) ;
#17083 = VECTOR ( 'NONE', #4166, 1000.000000000000000 ) ;
#17084 = DIRECTION ( 'NONE',  ( 1.000000000000000000, 5.889072920838430686E-16, -0.000000000000000000 ) ) ;
#17085 = MECHANICAL_DESIGN_GEOMETRIC_PRESENTATION_REPRESENTATION (  '', ( #2590 ), #10836 ) ;
#17086 = VERTEX_POINT ( 'NONE', #19760 ) ;
#17087 = CARTESIAN_POINT ( 'NONE',  ( 423.8334540492694487, 191.8198460455371333, 178.2339398819846110 ) ) ;
#17088 = CARTESIAN_POINT ( 'NONE',  ( -44.50085094405407915, 175.4489062796178871, 505.3921618609452935 ) ) ;
#17089 =( NAMED_UNIT ( * ) PLANE_ANGLE_UNIT ( ) SI_UNIT ( $, .RADIAN. ) );
#17090 = SURFACE_STYLE_USAGE ( .BOTH. , #19863 ) ;
#17091 = FACE_OUTER_BOUND ( 'NONE', #15172, .T. ) ;
#17092 = LINE ( 'NONE', #13795, #7935 ) ;
#17093 = VECTOR ( 'NONE', #5946, 1000.000000000000000 ) ;
#17094 = AXIS2_PLACEMENT_3D ( 'NONE', #18059, #19797, #10447 ) ;
#17095 = EDGE_CURVE ( 'NONE', #16181, #17448, #7617, .T. ) ;
#17096 = ORIENTED_EDGE ( 'NONE', *, *, #16650, .T. ) ;
#17097 = ORIENTED_EDGE ( 'NONE', *, *, #13584, .F. ) ;
#17098 = ORIENTED_EDGE ( 'NONE', *, *, #476, .F. ) ;
#17099 = EDGE_CURVE ( 'NONE', #5525, #18451, #17092, .T. ) ;
#17100 = ORIENTED_EDGE ( 'NONE', *, *, #3857, .T. ) ;
#17101 = ORIENTED_EDGE ( 'NONE', *, *, #399, .T. ) ;
#17102 = VERTEX_POINT ( 'NONE', #7223 ) ;
#17103 = SURFACE_SIDE_STYLE ('',( #10823 ) ) ;
#17104 = CARTESIAN_POINT ( 'NONE',  ( 1.000000000001310063, 139.7703989349544145, 489.5655098179835818 ) ) ;
#17105 = STYLED_ITEM ( 'NONE', ( #20354 ), #16452 ) ;
#17106 = CARTESIAN_POINT ( 'NONE',  ( -31.00000000000000000, 19.00000000000000000, -31.00000000000000000 ) ) ;
#17107 = VECTOR ( 'NONE', #10267, 1000.000000000000000 ) ;
#17108 = ORIENTED_EDGE ( 'NONE', *, *, #13185, .F. ) ;
#17109 =( NAMED_UNIT ( * ) SI_UNIT ( $, .STERADIAN. ) SOLID_ANGLE_UNIT ( ) );
#17110 = AXIS2_PLACEMENT_3D ( 'NONE', #17233, #6125, #12289 ) ;
#17111 = CARTESIAN_POINT ( 'NONE',  ( -23.00000000000002487, 10.00000000000000000, -31.00000000000003553 ) ) ;
#17112 = CARTESIAN_POINT ( 'NONE',  ( 53.48937290013659407, 209.5175665826582474, 345.1990110167342891 ) ) ;
#17113 = ORIENTED_EDGE ( 'NONE', *, *, #11908, .T. ) ;
#17114 = CARTESIAN_POINT ( 'NONE',  ( -34.99999999999999289, 8.000000000000000000, 35.00000000000000711 ) ) ;
#17115 = FILL_AREA_STYLE ('',( #13825 ) ) ;
#17116 = FILL_AREA_STYLE_COLOUR ( '', #6091 ) ;
#17117 = VECTOR ( 'NONE', #18225, 1000.000000000000000 ) ;
#17118 = AXIS2_PLACEMENT_3D ( 'NONE', #892, #8539, #7016 ) ;
#17119 = CIRCLE ( 'NONE', #12865, 3.000000000000000000 ) ;
#17120 = ORIENTED_EDGE ( 'NONE', *, *, #5695, .T. ) ;
#17121 = EDGE_CURVE ( 'NONE', #10263, #6022, #7919, .T. ) ;
#17122 = DIRECTION ( 'NONE',  ( 0.000000000000000000, -1.000000000000000000, 0.000000000000000000 ) ) ;
#17123 = STYLED_ITEM ( 'NONE', ( #19656 ), #11879 ) ;
#17124 = ORIENTED_EDGE ( 'NONE', *, *, #17534, .F. ) ;
#17125 = CARTESIAN_POINT ( 'NONE',  ( -37.00000000000000000, 68.00000000000000000, -22.99999999999999645 ) ) ;
#17126 = DIRECTION ( 'NONE',  ( -1.000000000000000000, -2.135044278125301096E-16, -0.000000000000000000 ) ) ;
#17127 = VERTEX_POINT ( 'NONE', #20068 ) ;
#17128 = PRESENTATION_STYLE_ASSIGNMENT (( #10848 ) ) ;
#17129 = FACE_OUTER_BOUND ( 'NONE', #16120, .T. ) ;
#17130 = CARTESIAN_POINT ( 'NONE',  ( -39.99999999999999289, 8.000000000000000000, 34.99999999999997868 ) ) ;
#17131 = VECTOR ( 'NONE', #10455, 1000.000000000000000 ) ;
#17132 = FACE_BOUND ( 'NONE', #2544, .T. ) ;
#17133 = CIRCLE ( 'NONE', #18439, 10.00000000000000888 ) ;
#17134 = DIRECTION ( 'NONE',  ( 0.000000000000000000, 0.000000000000000000, -1.000000000000000000 ) ) ;
#17135 = LINE ( 'NONE', #10754, #18440 ) ;
#17136 = CARTESIAN_POINT ( 'NONE',  ( 493.8117674897343363, 214.2156642432025251, 245.0000000000000000 ) ) ;
#17137 = ORIENTED_EDGE ( 'NONE', *, *, #19476, .F. ) ;
#17138 = DIRECTION ( 'NONE',  ( 1.000000000000000000, 0.000000000000000000, -1.322948291343117631E-12 ) ) ;
#17139 = FILL_AREA_STYLE_COLOUR ( '', #25 ) ;
#17140 =( LENGTH_UNIT ( ) NAMED_UNIT ( * ) SI_UNIT ( .MILLI., .METRE. ) );
#17141 = PRODUCT_DEFINITION_SHAPE ( 'NONE', 'NONE',  #14255 ) ;
#17142 = ORIENTED_EDGE ( 'NONE', *, *, #9289, .T. ) ;
#17143 = CARTESIAN_POINT ( 'NONE',  ( 463.8334540492693350, 191.8198460455371333, 24.99421986894476078 ) ) ;
#17144 = EDGE_CURVE ( 'NONE', #16810, #17234, #9236, .T. ) ;
#17145 = ORIENTED_EDGE ( 'NONE', *, *, #890, .F. ) ;
#17146 = ORIENTED_EDGE ( 'NONE', *, *, #14145, .T. ) ;
#17147 = ORIENTED_EDGE ( 'NONE', *, *, #13349, .F. ) ;
#17148 = MECHANICAL_DESIGN_GEOMETRIC_PRESENTATION_REPRESENTATION (  '', ( #2671 ), #7609 ) ;
#17149 = AXIS2_PLACEMENT_3D ( 'NONE', #6501, #1421, #11225 ) ;
#17150 = DIRECTION ( 'NONE',  ( 0.000000000000000000, 0.000000000000000000, 1.000000000000000000 ) ) ;
#17151 = VERTEX_POINT ( 'NONE', #2668 ) ;
#17152 = DIRECTION ( 'NONE',  ( 0.000000000000000000, 0.000000000000000000, 1.000000000000000000 ) ) ;
#17153 = VERTEX_POINT ( 'NONE', #4140 ) ;
#17154 = LINE ( 'NONE', #14072, #9388 ) ;
#17155 = ADVANCED_FACE ( 'NONE', ( #5664 ), #12154, .T. ) ;
#17156 = CARTESIAN_POINT ( 'NONE',  ( 45.00000000000001421, 0.000000000000000000, -150.0000000000000000 ) ) ;
#17157 = LINE ( 'NONE', #1165, #491 ) ;
#17158 = CARTESIAN_POINT ( 'NONE',  ( -3.000000000000000000, 6.000000000000000000, 3.000000000000000000 ) ) ;
#17159 = EDGE_CURVE ( 'NONE', #6498, #8554, #11568, .T. ) ;
#17160 = ORIENTED_EDGE ( 'NONE', *, *, #791, .F. ) ;
#17161 = CYLINDRICAL_SURFACE ( 'NONE', #7520, 8.000000000000000000 ) ;
#17162 = DIRECTION ( 'NONE',  ( -1.000000000000000000, -1.595148023886719315E-16, 0.000000000000000000 ) ) ;
#17163 =( GEOMETRIC_REPRESENTATION_CONTEXT ( 3 ) GLOBAL_UNCERTAINTY_ASSIGNED_CONTEXT ( ( #7632 ) ) GLOBAL_UNIT_ASSIGNED_CONTEXT ( ( #9447, #265, #3046 ) ) REPRESENTATION_CONTEXT ( 'NONE', 'WORKASPACE' ) );
#17164 = CARTESIAN_POINT ( 'NONE',  ( -1.000000000000014655, 152.4824555358011082, 486.3411705753778165 ) ) ;
#17165 = CARTESIAN_POINT ( 'NONE',  ( 78.48937290013662960, 1.675782865040797740E-14, 0.000000000000000000 ) ) ;
#17166 = DIRECTION ( 'NONE',  ( 0.000000000000000000, 0.000000000000000000, -1.000000000000000000 ) ) ;
#17167 = CARTESIAN_POINT ( 'NONE',  ( -1.000000000000012657, 139.1177163613726577, 488.5223183823763407 ) ) ;
#17168 = AXIS2_PLACEMENT_3D ( 'NONE', #2530, #2315, #15109 ) ;
#17169 = FILL_AREA_STYLE_COLOUR ( '', #639 ) ;
#17170 = ORIENTED_EDGE ( 'NONE', *, *, #17159, .T. ) ;
#17171 = VERTEX_POINT ( 'NONE', #2770 ) ;
#17172 = ADVANCED_FACE ( 'NONE', ( #13896 ), #15527, .T. ) ;
#17173 = ORIENTED_EDGE ( 'NONE', *, *, #14923, .F. ) ;
#17174 = EDGE_LOOP ( 'NONE', ( #12567, #12187, #15150, #9441 ) ) ;
#17175 = CARTESIAN_POINT ( 'NONE',  ( 26.00000000000000000, 19.00000000000000000, 40.00000000000001421 ) ) ;
#17176 = STYLED_ITEM ( 'NONE', ( #18595 ), #17818 ) ;
#17177 = ORIENTED_EDGE ( 'NONE', *, *, #12093, .F. ) ;
#17178 = CARTESIAN_POINT ( 'NONE',  ( -211.5106270998635409, 123.1299228374912644, 220.6387154965113382 ) ) ;
#17179 = EDGE_CURVE ( 'NONE', #16123, #9243, #12369, .T. ) ;
#17180 = CARTESIAN_POINT ( 'NONE',  ( 53.48937290013658696, 122.8810204491430369, 322.0399576098686225 ) ) ;
#17181 = PRESENTATION_LAYER_ASSIGNMENT (  '', '', ( #12239 ) ) ;
#17182 = VERTEX_POINT ( 'NONE', #10503 ) ;
#17183 = SURFACE_SIDE_STYLE ('',( #15453 ) ) ;
#17184 = CARTESIAN_POINT ( 'NONE',  ( 30.99999999999999645, 3.000000000000000000, 26.00000000000000355 ) ) ;
#17185 = DIRECTION ( 'NONE',  ( 0.000000000000000000, 1.000000000000000000, 0.000000000000000000 ) ) ;
#17186 =( LENGTH_UNIT ( ) NAMED_UNIT ( * ) SI_UNIT ( .MILLI., .METRE. ) );
#17187 = PRESENTATION_LAYER_ASSIGNMENT (  '', '', ( #6344 ) ) ;
#17188 = ADVANCED_FACE ( 'NONE', ( #12072 ), #7524, .T. ) ;
#17189 = LINE ( 'NONE', #19021, #11117 ) ;
#17190 = DIRECTION ( 'NONE',  ( 6.123031769111888756E-17, 0.000000000000000000, 1.000000000000000000 ) ) ;
#17191 = CYLINDRICAL_SURFACE ( 'NONE', #5298, 2.500000000000002220 ) ;
#17192 = EDGE_CURVE ( 'NONE', #4894, #2001, #14013, .T. ) ;
#17193 = DIRECTION ( 'NONE',  ( 0.000000000000000000, -0.000000000000000000, 1.000000000000000000 ) ) ;
#17194 = AXIS2_PLACEMENT_3D ( 'NONE', #19613, #5222, #16264 ) ;
#17195 = CARTESIAN_POINT ( 'NONE',  ( 25.99999999999997868, 10.00000000000000000, 40.00000000000000711 ) ) ;
#17196 = VECTOR ( 'NONE', #16291, 1000.000000000000000 ) ;
#17197 = AXIS2_PLACEMENT_3D ( 'NONE', #4699, #6260, #13984 ) ;
#17198 = EDGE_CURVE ( 'NONE', #11810, #10797, #7726, .T. ) ;
#17199 = EDGE_CURVE ( 'NONE', #11163, #13735, #3076, .T. ) ;
#17200 = ORIENTED_EDGE ( 'NONE', *, *, #473, .T. ) ;
#17201 = ORIENTED_EDGE ( 'NONE', *, *, #2053, .T. ) ;
#17202 = ORIENTED_EDGE ( 'NONE', *, *, #12912, .F. ) ;
#17203 = VECTOR ( 'NONE', #10528, 1000.000000000000000 ) ;
#17204 = SURFACE_STYLE_USAGE ( .BOTH. , #15691 ) ;
#17205 = ORIENTED_EDGE ( 'NONE', *, *, #5949, .F. ) ;
#17206 = VECTOR ( 'NONE', #14339, 1000.000000000000000 ) ;
#17207 = ORIENTED_EDGE ( 'NONE', *, *, #1560, .F. ) ;
#17208 = ORIENTED_EDGE ( 'NONE', *, *, #10572, .F. ) ;
#17209 = DIRECTION ( 'NONE',  ( 1.450371633464474201E-15, 0.000000000000000000, 1.000000000000000000 ) ) ;
#17210 = CARTESIAN_POINT ( 'NONE',  ( 22.99999999999999645, 68.00000000000000000, 31.00000000000006750 ) ) ;
#17211 = CIRCLE ( 'NONE', #19823, 15.14120580695350071 ) ;
#17212 = AXIS2_PLACEMENT_3D ( 'NONE', #14387, #8210, #14177 ) ;
#17213 =( LENGTH_UNIT ( ) NAMED_UNIT ( * ) SI_UNIT ( .MILLI., .METRE. ) );
#17214 = DIRECTION ( 'NONE',  ( 0.000000000000000000, 0.000000000000000000, -1.000000000000000000 ) ) ;
#17215 = LINE ( 'NONE', #7453, #6364 ) ;
#17216 = SURFACE_STYLE_FILL_AREA ( #14035 ) ;
#17217 = CARTESIAN_POINT ( 'NONE',  ( -26.00000000000000000, 11.00000000000000000, -31.00000000000003908 ) ) ;
#17218 = CARTESIAN_POINT ( 'NONE',  ( 98.48937290013662960, 113.1299228374914350, 220.6387154965113382 ) ) ;
#17219 = CLOSED_SHELL ( 'NONE', ( #17818, #19095, #2851, #3975, #170, #13523 ) ) ;
#17220 = VERTEX_POINT ( 'NONE', #11213 ) ;
#17221 = DIRECTION ( 'NONE',  ( 0.000000000000000000, 1.000000000000000000, -0.000000000000000000 ) ) ;
#17222 = EDGE_CURVE ( 'NONE', #63, #14745, #15998, .T. ) ;
#17223 = DIRECTION ( 'NONE',  ( -1.000000000000000000, 0.000000000000000000, 0.000000000000000000 ) ) ;
#17224 = ADVANCED_FACE ( 'NONE', ( #15877 ), #11118, .T. ) ;
#17225 = AXIS2_PLACEMENT_3D ( 'NONE', #11338, #4956, #8356 ) ;
#17226 = AXIS2_PLACEMENT_3D ( 'NONE', #18168, #16667, #12300 ) ;
#17227 = EDGE_CURVE ( 'NONE', #2567, #2573, #17614, .T. ) ;
#17228 = VERTEX_POINT ( 'NONE', #9671 ) ;
#17229 =( GEOMETRIC_REPRESENTATION_CONTEXT ( 3 ) GLOBAL_UNCERTAINTY_ASSIGNED_CONTEXT ( ( #8895 ) ) GLOBAL_UNIT_ASSIGNED_CONTEXT ( ( #18791, #10979, #11179 ) ) REPRESENTATION_CONTEXT ( 'NONE', 'WORKASPACE' ) );
#17230 = DIRECTION ( 'NONE',  ( 1.000000000000000000, 0.000000000000000000, 0.000000000000000000 ) ) ;
#17231 = AXIS2_PLACEMENT_3D ( 'NONE', #7144, #13430, #19668 ) ;
#17232 = ORIENTED_EDGE ( 'NONE', *, *, #10541, .T. ) ;
#17233 = CARTESIAN_POINT ( 'NONE',  ( 133.4893729001365728, 0.000000000000000000, -97.94896630388704750 ) ) ;
#17234 = VERTEX_POINT ( 'NONE', #12466 ) ;
#17235 = CARTESIAN_POINT ( 'NONE',  ( 178.4893729001365443, 145.9162550801369491, 250.0000000000000000 ) ) ;
#17236 = CARTESIAN_POINT ( 'NONE',  ( 111.4893729001366012, 129.7247684487574304, 252.0000000000000000 ) ) ;
#17237 = SURFACE_STYLE_USAGE ( .BOTH. , #14052 ) ;
#17238 = ADVANCED_BREP_SHAPE_REPRESENTATION ( '', ( #8261, #8166, #2741 ), #5024 ) ;
#17239 =( GEOMETRIC_REPRESENTATION_CONTEXT ( 3 ) GLOBAL_UNCERTAINTY_ASSIGNED_CONTEXT ( ( #2257 ) ) GLOBAL_UNIT_ASSIGNED_CONTEXT ( ( #17186, #12363, #7917 ) ) REPRESENTATION_CONTEXT ( 'NONE', 'WORKASPACE' ) );
#17240 = VECTOR ( 'NONE', #16647, 1000.000000000000000 ) ;
#17241 = FILL_AREA_STYLE_COLOUR ( '', #4799 ) ;
#17242 = DIRECTION ( 'NONE',  ( -0.000000000000000000, -1.000000000000000000, -0.000000000000000000 ) ) ;
#17243 = DIRECTION ( 'NONE',  ( 1.000000000000000000, 0.000000000000000000, 0.000000000000000000 ) ) ;
#17244 = MECHANICAL_DESIGN_GEOMETRIC_PRESENTATION_REPRESENTATION (  '', ( #11990 ), #10999 ) ;
#17245 = FILL_AREA_STYLE ('',( #12505 ) ) ;
#17246 = EDGE_LOOP ( 'NONE', ( #4433, #7441, #15604, #500 ) ) ;
#17247 = CARTESIAN_POINT ( 'NONE',  ( 53.48937290013659407, 210.4096692328538154, 345.9586017849865129 ) ) ;
#17248 = CARTESIAN_POINT ( 'NONE',  ( 111.4893729001366012, 127.7247684487574588, 357.7985149490353933 ) ) ;
#17249 = PRODUCT_CONTEXT ( 'NONE', #1403, 'mechanical' ) ;
#17250 = EDGE_CURVE ( 'NONE', #16622, #10073, #3323, .T. ) ;
#17251 = ORIENTED_EDGE ( 'NONE', *, *, #14536, .T. ) ;
#17252 = CARTESIAN_POINT ( 'NONE',  ( 25.99999999999998224, 10.00000000000000000, -31.00000000000003197 ) ) ;
#17253 = VERTEX_POINT ( 'NONE', #19139 ) ;
#17254 = CIRCLE ( 'NONE', #18230, 4.999999999999997335 ) ;
#17255 = EDGE_LOOP ( 'NONE', ( #12784, #13422, #5885, #3902, #17498, #16222 ) ) ;
#17256 = ORIENTED_EDGE ( 'NONE', *, *, #10094, .T. ) ;
#17257 = MECHANICAL_DESIGN_GEOMETRIC_PRESENTATION_REPRESENTATION (  '', ( #4101 ), #6090 ) ;
#17258 = VECTOR ( 'NONE', #6014, 1000.000000000000000 ) ;
#17259 = LINE ( 'NONE', #9615, #9730 ) ;
#17260 = VECTOR ( 'NONE', #16618, 1000.000000000000000 ) ;
#17261 = EDGE_LOOP ( 'NONE', ( #2309, #3815, #18416, #3906 ) ) ;
#17262 = LINE ( 'NONE', #1787, #19871 ) ;
#17263 = VERTEX_POINT ( 'NONE', #4632 ) ;
#17264 = LINE ( 'NONE', #17063, #10055 ) ;
#17265 = CYLINDRICAL_SURFACE ( 'NONE', #4696, 2.999999999999995559 ) ;
#17266 = VECTOR ( 'NONE', #9550, 1000.000000000000114 ) ;
#17267 = CARTESIAN_POINT ( 'NONE',  ( 0.000000000000000000, 341.0487089519837696, -115.0000000000032969 ) ) ;
#17268 = AXIS2_PLACEMENT_3D ( 'NONE', #4465, #20218, #19999 ) ;
#17269 = CARTESIAN_POINT ( 'NONE',  ( -80.17878486073050226, 139.8636771835041372, 489.1515118754280138 ) ) ;
#17270 = FACE_OUTER_BOUND ( 'NONE', #10180, .T. ) ;
#17271 = CARTESIAN_POINT ( 'NONE',  ( -75.00000000000000000, 313.8311070602663904, -87.78239810828596035 ) ) ;
#17272 = FACE_OUTER_BOUND ( 'NONE', #18286, .T. ) ;
#17273 = ORIENTED_EDGE ( 'NONE', *, *, #5374, .T. ) ;
#17274 = DIRECTION ( 'NONE',  ( -0.000000000000000000, -1.000000000000000000, -0.000000000000000000 ) ) ;
#17275 = DIRECTION ( 'NONE',  ( 0.000000000000000000, 0.000000000000000000, 1.000000000000000000 ) ) ;
#17276 = DIRECTION ( 'NONE',  ( 1.000000000000000000, 0.000000000000000000, 0.000000000000000000 ) ) ;
#17277 = CARTESIAN_POINT ( 'NONE',  ( -35.00000000000000000, 19.00000000000000000, 20.99999999999999289 ) ) ;
#17278 = DIRECTION ( 'NONE',  ( 1.000000000000000000, 5.889072920838430686E-16, -0.000000000000000000 ) ) ;
#17279 = COLOUR_RGB ( '', 0.72549020, 0.75294118, 0.79215686) ;
#17280 = LINE ( 'NONE', #12539, #16525 ) ;
#17281 = VERTEX_POINT ( 'NONE', #3188 ) ;
#17282 = ADVANCED_FACE ( 'NONE', ( #9370 ), #5046, .T. ) ;
#17283 = COLOUR_RGB ( '', 0.66274510, 0.83137255, 0.94901961) ;
#17284 = ORIENTED_EDGE ( 'NONE', *, *, #14272, .F. ) ;
#17285 = PRODUCT_DEFINITION ( 'UNKNOWN', '', #17850, #14818 ) ;
#17286 = VERTEX_POINT ( 'NONE', #12677 ) ;
#17287 = FACE_OUTER_BOUND ( 'NONE', #18884, .T. ) ;
#17288 = CARTESIAN_POINT ( 'NONE',  ( -80.03794136217337041, 139.6076487680217042, 500.4896316014566651 ) ) ;
#17289 = ORIENTED_EDGE ( 'NONE', *, *, #7030, .F. ) ;
#17290 = FILL_AREA_STYLE ('',( #3057 ) ) ;
#17291 = STYLED_ITEM ( 'NONE', ( #13526 ), #14951 ) ;
#17292 = ORIENTED_EDGE ( 'NONE', *, *, #14272, .T. ) ;
#17293 = ADVANCED_FACE ( 'NONE', ( #1606 ), #10910, .T. ) ;
#17294 = FACE_BOUND ( 'NONE', #4172, .T. ) ;
#17295 = CYLINDRICAL_SURFACE ( 'NONE', #4684, 2.000000000000001776 ) ;
#17296 = PRESENTATION_LAYER_ASSIGNMENT (  '', '', ( #4801 ) ) ;
#17297 = SURFACE_STYLE_USAGE ( .BOTH. , #9871 ) ;
#17298 = CARTESIAN_POINT ( 'NONE',  ( -2.693790225569811625, 61.33495048777871261, 9.110418847747206783 ) ) ;
#17299 = DIRECTION ( 'NONE',  ( 0.000000000000000000, 1.000000000000000000, 0.000000000000000000 ) ) ;
#17300 = AXIS2_PLACEMENT_3D ( 'NONE', #2829, #20128, #12837 ) ;
#17301 = PLANE ( 'NONE',  #19188 ) ;
#17302 = CARTESIAN_POINT ( 'NONE',  ( -37.00000000000000000, 0.000000000000000000, 23.00000000000000355 ) ) ;
#17303 = CARTESIAN_POINT ( 'NONE',  ( -22.99999999999999645, 68.00000000000000000, 37.00000000000002132 ) ) ;
#17304 = CARTESIAN_POINT ( 'NONE',  ( -40.00000000000000000, 0.000000000000000000, 26.00000000000000355 ) ) ;
#17305 = PLANE ( 'NONE',  #4739 ) ;
#17306 = EDGE_CURVE ( 'NONE', #2001, #7513, #12555, .T. ) ;
#17307 = ORIENTED_EDGE ( 'NONE', *, *, #20216, .T. ) ;
#17308 = EDGE_LOOP ( 'NONE', ( #16443, #7714, #5690, #4795 ) ) ;
#17309 = AXIS2_PLACEMENT_3D ( 'NONE', #15891, #3203, #7940 ) ;
#17310 = EDGE_CURVE ( 'NONE', #19125, #17405, #5326, .T. ) ;
#17311 = FACE_OUTER_BOUND ( 'NONE', #11229, .T. ) ;
#17312 = ORIENTED_EDGE ( 'NONE', *, *, #19850, .T. ) ;
#17313 = ORIENTED_EDGE ( 'NONE', *, *, #3445, .F. ) ;
#17314 = ORIENTED_EDGE ( 'NONE', *, *, #18890, .T. ) ;
#17315 = LINE ( 'NONE', #19151, #203 ) ;
#17316 = VECTOR ( 'NONE', #17406, 1000.000000000000000 ) ;
#17317 = ADVANCED_FACE ( 'NONE', ( #4937 ), #6290, .F. ) ;
#17318 = CARTESIAN_POINT ( 'NONE',  ( -58.16843972078500258, 319.7545334744432353, 485.1700099148404206 ) ) ;
#17319 = CARTESIAN_POINT ( 'NONE',  ( -31.00000000000005684, 10.00000000000000000, -23.00000000000000000 ) ) ;
#17320 = DIRECTION ( 'NONE',  ( 1.000000000000000000, 0.000000000000000000, -0.000000000000000000 ) ) ;
#17321 = EDGE_CURVE ( 'NONE', #12399, #19270, #7002, .T. ) ;
#17322 = FACE_OUTER_BOUND ( 'NONE', #5551, .T. ) ;
#17323 = PRODUCT ( 'Servo-Bas', 'Servo-Bas', '', ( #10762 ) ) ;
#17324 = LINE ( 'NONE', #1738, #18524 ) ;
#17325 = EDGE_CURVE ( 'NONE', #3980, #8032, #3602, .T. ) ;
#17326 = CARTESIAN_POINT ( 'NONE',  ( 31.00000000000000000, 11.00000000000000000, 30.99999999999999289 ) ) ;
#17327 = AXIS2_PLACEMENT_3D ( 'NONE', #2660, #7425, #10806 ) ;
#17328 = ORIENTED_EDGE ( 'NONE', *, *, #691, .T. ) ;
#17329 = CARTESIAN_POINT ( 'NONE',  ( -32.00000000000000711, 6.000000000000000000, -22.00000000000000355 ) ) ;
#17330 = CARTESIAN_POINT ( 'NONE',  ( 1.399999999999999911, 0.000000000000000000, 0.000000000000000000 ) ) ;
#17331 = AXIS2_PLACEMENT_3D ( 'NONE', #9861, #12765, #8013 ) ;
#17332 = EDGE_CURVE ( 'NONE', #13294, #6379, #1319, .T. ) ;
#17333 = ORIENTED_EDGE ( 'NONE', *, *, #8799, .T. ) ;
#17334 = DIRECTION ( 'NONE',  ( 0.000000000000000000, 1.000000000000000000, 0.000000000000000000 ) ) ;
#17335 = ORIENTED_EDGE ( 'NONE', *, *, #8756, .T. ) ;
#17336 = EDGE_CURVE ( 'NONE', #9984, #13589, #11430, .T. ) ;
#17337 = CYLINDRICAL_SURFACE ( 'NONE', #3450, 1.999999999999997113 ) ;
#17338 = DIRECTION ( 'NONE',  ( 0.000000000000000000, 1.000000000000000000, 0.000000000000000000 ) ) ;
#17339 = ORIENTED_EDGE ( 'NONE', *, *, #18314, .F. ) ;
#17340 = SURFACE_SIDE_STYLE ('',( #6848 ) ) ;
#17341 = DIRECTION ( 'NONE',  ( 1.000000000000000000, 0.000000000000000000, 0.000000000000000000 ) ) ;
#17342 =( LENGTH_UNIT ( ) NAMED_UNIT ( * ) SI_UNIT ( .MILLI., .METRE. ) );
#17343 = CARTESIAN_POINT ( 'NONE',  ( 0.3141013587250581218, 139.8869819025744334, 501.0706778502146790 ) ) ;
#17344 = CARTESIAN_POINT ( 'NONE',  ( 30.99999999999999645, 68.00000000000000000, 26.00000000000001066 ) ) ;
#17345 = CARTESIAN_POINT ( 'NONE',  ( 31.00000000000000000, 19.00000000000000000, -31.00000000000000355 ) ) ;
#17346 = CARTESIAN_POINT ( 'NONE',  ( 9.796850830579020038E-16, 6.000000000000000000, 22.00000000000000000 ) ) ;
#17347 = VERTEX_POINT ( 'NONE', #14511 ) ;
#17348 = FACE_OUTER_BOUND ( 'NONE', #14878, .T. ) ;
#17349 = FILL_AREA_STYLE ('',( #17139 ) ) ;
#17351 = ORIENTED_EDGE ( 'NONE', *, *, #2342, .F. ) ;
#17350 = MECHANICAL_DESIGN_GEOMETRIC_PRESENTATION_REPRESENTATION (  '', ( #18331 ), #14726 ) ;
#17352 = SPHERICAL_SURFACE ( 'NONE', #16224, 1.000000000000000000 ) ;
#17353 = ORIENTED_EDGE ( 'NONE', *, *, #68, .F. ) ;
#17355 = EDGE_LOOP ( 'NONE', ( #11721, #13000, #18433, #13934 ) ) ;
#17354 = SHAPE_REPRESENTATION ( 'Servo-Body.2', ( #2741 ), #3403 ) ;
#17356 = EDGE_CURVE ( 'NONE', #11627, #9383, #6814, .T. ) ;
#17357 = ORIENTED_EDGE ( 'NONE', *, *, #10134, .T. ) ;
#17358 =( NAMED_UNIT ( * ) PLANE_ANGLE_UNIT ( ) SI_UNIT ( $, .RADIAN. ) );
#17359 = EDGE_LOOP ( 'NONE', ( #14348, #14934, #20335, #2317 ) ) ;
#17360 = MECHANICAL_DESIGN_GEOMETRIC_PRESENTATION_REPRESENTATION (  '', ( #12101 ), #18992 ) ;
#17361 = CARTESIAN_POINT ( 'NONE',  ( 0.000000000000000000, 10.00000000000000000, -12.00000000000000178 ) ) ;
#17362 = CARTESIAN_POINT ( 'NONE',  ( 143.0892156028631348, 80.91625508013694912, 250.0000000000000000 ) ) ;
#17363 = ORIENTED_EDGE ( 'NONE', *, *, #399, .F. ) ;
#17364 = FILL_AREA_STYLE_COLOUR ( '', #19166 ) ;
#17365 = VECTOR ( 'NONE', #11619, 1000.000000000000000 ) ;
#17366 = DIRECTION ( 'NONE',  ( 0.000000000000000000, -1.000000000000000000, 0.000000000000000000 ) ) ;
#17367 = FACE_OUTER_BOUND ( 'NONE', #17056, .T. ) ;
#17368 = PLANE ( 'NONE',  #14001 ) ;
#17369 = DIRECTION ( 'NONE',  ( 0.000000000000000000, -1.000000000000000000, 0.000000000000000000 ) ) ;
#17370 = SURFACE_STYLE_USAGE ( .BOTH. , #13980 ) ;
#17371 = ORIENTED_EDGE ( 'NONE', *, *, #13768, .F. ) ;
#17372 = PLANE ( 'NONE',  #8632 ) ;
#17373 = CARTESIAN_POINT ( 'NONE',  ( 31.00000000000003553, 10.00000000000000000, -22.99999999999999645 ) ) ;
#17374 = CARTESIAN_POINT ( 'NONE',  ( 1.181929469892505358, 138.7723821175183048, 490.5025619656410640 ) ) ;
#17375 =( LENGTH_UNIT ( ) NAMED_UNIT ( * ) SI_UNIT ( .MILLI., .METRE. ) );
#17376 = DIRECTION ( 'NONE',  ( -1.595148023886719315E-16, 1.000000000000000000, -0.000000000000000000 ) ) ;
#17377 = DIRECTION ( 'NONE',  ( 0.000000000000000000, -1.000000000000000000, 0.000000000000000000 ) ) ;
#17378 = DIRECTION ( 'NONE',  ( 1.632680918566406990E-15, -0.7817866094812271349, -0.6235460666509309302 ) ) ;
#17379 = CARTESIAN_POINT ( 'NONE',  ( 0.000000000000000000, 80.91625508013694912, 0.000000000000000000 ) ) ;
#17380 = VERTEX_POINT ( 'NONE', #17908 ) ;
#17381 = VECTOR ( 'NONE', #1065, 1000.000000000000000 ) ;
#17382 = ORIENTED_EDGE ( 'NONE', *, *, #15797, .F. ) ;
#17383 = DIRECTION ( 'NONE',  ( -1.000000000000000000, 0.000000000000000000, 0.000000000000000000 ) ) ;
#17384 = CARTESIAN_POINT ( 'NONE',  ( -80.71241711305556521, 140.4313724365906353, 500.8555218219611334 ) ) ;
#17385 = ORIENTED_EDGE ( 'NONE', *, *, #9257, .F. ) ;
#17386 = ADVANCED_FACE ( 'NONE', ( #5346 ), #12993, .F. ) ;
#17387 = ORIENTED_EDGE ( 'NONE', *, *, #13676, .F. ) ;
#17388 = CYLINDRICAL_SURFACE ( 'NONE', #5270, 4.000000000000003553 ) ;
#17389 = DIRECTION ( 'NONE',  ( 0.000000000000000000, 0.000000000000000000, 1.000000000000000000 ) ) ;
#17390 = FACE_OUTER_BOUND ( 'NONE', #4189, .T. ) ;
#17391 = COLOUR_RGB ( '', 0.66274510, 0.83137255, 0.94901961) ;
#17392 = FACE_OUTER_BOUND ( 'NONE', #422, .T. ) ;
#17393 = DIRECTION ( 'NONE',  ( 0.000000000000000000, 1.000000000000000000, 0.000000000000000000 ) ) ;
#17394 = LINE ( 'NONE', #11114, #8900 ) ;
#17395 = CARTESIAN_POINT ( 'NONE',  ( 36.99999999999999289, 10.00000000000000000, 22.99999999999999645 ) ) ;
#17396 = CARTESIAN_POINT ( 'NONE',  ( 108.9893729001365870, 143.5567736071463969, 294.7336993003747239 ) ) ;
#17397 = FILL_AREA_STYLE_COLOUR ( '', #8872 ) ;
#17398 = ADVANCED_FACE ( 'NONE', ( #5545 ), #14927, .F. ) ;
#17399 = ORIENTED_EDGE ( 'NONE', *, *, #4070, .F. ) ;
#17400 = ORIENTED_EDGE ( 'NONE', *, *, #4195, .T. ) ;
#17401 = AXIS2_PLACEMENT_3D ( 'NONE', #15995, #1916, #2892 ) ;
#17402 =( LENGTH_UNIT ( ) NAMED_UNIT ( * ) SI_UNIT ( .MILLI., .METRE. ) );
#17403 = ORIENTED_EDGE ( 'NONE', *, *, #2184, .T. ) ;
#17404 = ORIENTED_EDGE ( 'NONE', *, *, #17667, .T. ) ;
#17405 = VERTEX_POINT ( 'NONE', #1917 ) ;
#17406 = DIRECTION ( 'NONE',  ( 1.000000000000000000, -0.000000000000000000, -0.000000000000000000 ) ) ;
#17407 = DIRECTION ( 'NONE',  ( 0.000000000000000000, -1.000000000000000000, 0.000000000000000000 ) ) ;
#17408 = DIRECTION ( 'NONE',  ( 0.000000000000000000, 0.000000000000000000, -1.000000000000000000 ) ) ;
#17409 = CARTESIAN_POINT ( 'NONE',  ( -40.00000000000000000, 19.00000000000000000, 25.99999999999999645 ) ) ;
#17411 = EDGE_CURVE ( 'NONE', #9677, #12613, #10565, .T. ) ;
#17410 = CARTESIAN_POINT ( 'NONE',  ( -22.00000000000001776, 8.000000000000000000, 33.00000000000000711 ) ) ;
#17412 = SURFACE_SIDE_STYLE ('',( #17216 ) ) ;
#17413 = AXIS2_PLACEMENT_3D ( 'NONE', #18728, #6076, #18819 ) ;
#17414 = DIRECTION ( 'NONE',  ( 7.900838015626929923E-17, 8.586860021784410058E-33, -1.000000000000000000 ) ) ;
#17415 = DIRECTION ( 'NONE',  ( 1.000000000000000000, 0.000000000000000000, 0.000000000000000000 ) ) ;
#17416 = AXIS2_PLACEMENT_3D ( 'NONE', #9138, #7593, #20147 ) ;
#17417 = EDGE_CURVE ( 'NONE', #2260, #5553, #13290, .T. ) ;
#17418 = VERTEX_POINT ( 'NONE', #8628 ) ;
#17419 = ADVANCED_FACE ( 'NONE', ( #17805 ), #7109, .F. ) ;
#17420 = ORIENTED_EDGE ( 'NONE', *, *, #13584, .T. ) ;
#17421 = EDGE_CURVE ( 'NONE', #2723, #645, #8237, .T. ) ;
#17422 = VECTOR ( 'NONE', #1267, 1000.000000000000000 ) ;
#17423 = CIRCLE ( 'NONE', #5609, 18.49999999999998934 ) ;
#17424 = AXIS2_PLACEMENT_3D ( 'NONE', #13538, #15295, #18270 ) ;
#17425 = CYLINDRICAL_SURFACE ( 'NONE', #4966, 10.00000000000000888 ) ;
#17426 = ORIENTED_EDGE ( 'NONE', *, *, #14573, .T. ) ;
#17427 = PLANE ( 'NONE',  #16634 ) ;
#17428 = SURFACE_STYLE_FILL_AREA ( #7655 ) ;
#17429 = ORIENTED_EDGE ( 'NONE', *, *, #13736, .F. ) ;
#17430 = CARTESIAN_POINT ( 'NONE',  ( 0.000000000000000000, 219.7545334744432921, 515.1946179577817020 ) ) ;
#17431 = ADVANCED_FACE ( 'NONE', ( #2138 ), #884, .T. ) ;
#17432 = CARTESIAN_POINT ( 'NONE',  ( -1.214306433183764966E-14, 141.4538060686001302, 501.7130291278048162 ) ) ;
#17433 = DIRECTION ( 'NONE',  ( -1.000000000000000000, -2.135044278125301096E-16, -0.000000000000000000 ) ) ;
#17434 = DIRECTION ( 'NONE',  ( -1.000000000000000000, -0.000000000000000000, -0.000000000000000000 ) ) ;
#17435 = ORIENTED_EDGE ( 'NONE', *, *, #407, .F. ) ;
#17436 = CARTESIAN_POINT ( 'NONE',  ( -1.387778780781445676E-14, 138.7545334744432637, 489.5655098179848892 ) ) ;
#17437 = CARTESIAN_POINT ( 'NONE',  ( 3.000000000000000000, 1.836909530733565148E-16, 22.00000000000000000 ) ) ;
#17438 = DIRECTION ( 'NONE',  ( -1.000000000000000000, 0.000000000000000000, -5.782411586589400040E-16 ) ) ;
#17439 = CIRCLE ( 'NONE', #9892, 14.59999999999999964 ) ;
#17440 = PRODUCT_CONTEXT ( 'NONE', #16850, 'mechanical' ) ;
#17441 = EDGE_CURVE ( 'NONE', #17030, #3979, #10926, .T. ) ;
#17442 = VECTOR ( 'NONE', #10489, 1000.000000000000000 ) ;
#17443 = ORIENTED_EDGE ( 'NONE', *, *, #6247, .T. ) ;
#17444 = VERTEX_POINT ( 'NONE', #9140 ) ;
#17445 = EDGE_LOOP ( 'NONE', ( #1565, #14089, #14936, #5381 ) ) ;
#17446 = EDGE_CURVE ( 'NONE', #17263, #12727, #18403, .T. ) ;
#17447 = ORIENTED_EDGE ( 'NONE', *, *, #17690, .T. ) ;
#17448 = VERTEX_POINT ( 'NONE', #4109 ) ;
#17449 =( LENGTH_UNIT ( ) NAMED_UNIT ( * ) SI_UNIT ( .MILLI., .METRE. ) );
#17450 = ORIENTED_EDGE ( 'NONE', *, *, #12446, .F. ) ;
#17451 = DIRECTION ( 'NONE',  ( 0.000000000000000000, 0.000000000000000000, -1.000000000000000000 ) ) ;
#17452 = AXIS2_PLACEMENT_3D ( 'NONE', #5563, #6441, #19300 ) ;
#17453 = VERTEX_POINT ( 'NONE', #1071 ) ;
#17454 = DIRECTION ( 'NONE',  ( -0.000000000000000000, -1.000000000000000000, -0.000000000000000000 ) ) ;
#17455 = VECTOR ( 'NONE', #5496, 1000.000000000000000 ) ;
#17456 =( LENGTH_UNIT ( ) NAMED_UNIT ( * ) SI_UNIT ( .MILLI., .METRE. ) );
#17457 = DIRECTION ( 'NONE',  ( -0.000000000000000000, -1.000000000000000000, -0.000000000000000000 ) ) ;
#17458 = DIRECTION ( 'NONE',  ( 0.000000000000000000, 0.000000000000000000, -1.000000000000000000 ) ) ;
#17459 = CARTESIAN_POINT ( 'NONE',  ( -1.507804506096813046, 38.39915541515519237, 9.381017998102995747 ) ) ;
#17460 = AXIS2_PLACEMENT_3D ( 'NONE', #5271, #11546, #13602 ) ;
#17461 = EDGE_CURVE ( 'NONE', #16534, #5524, #10278, .T. ) ;
#17462 = EDGE_LOOP ( 'NONE', ( #7652, #17420, #1920, #3562 ) ) ;
#17463 = SURFACE_SIDE_STYLE ('',( #6785 ) ) ;
#17464 = CARTESIAN_POINT ( 'NONE',  ( 10.00000000000000000, 372.8685141053783241, -150.1198051533980049 ) ) ;
#17465 = DIRECTION ( 'NONE',  ( 0.000000000000000000, -1.000000000000000000, 0.000000000000000000 ) ) ;
#17466 = DIRECTION ( 'NONE',  ( -1.000000000000000000, 8.315472005415352149E-14, -1.318389841601051321E-12 ) ) ;
#17467 = CARTESIAN_POINT ( 'NONE',  ( 25.99999999999996092, 3.000000000000000000, 40.00000000000000711 ) ) ;
#17468 = CARTESIAN_POINT ( 'NONE',  ( 53.48937290013659407, 209.7811923590224978, 348.0151256184570343 ) ) ;
#17469 = EDGE_CURVE ( 'NONE', #10840, #18058, #4301, .T. ) ;
#17470 = VECTOR ( 'NONE', #1802, 1000.000000000000000 ) ;
#17471 = ORIENTED_EDGE ( 'NONE', *, *, #19660, .F. ) ;
#17472 = AXIS2_PLACEMENT_3D ( 'NONE', #11318, #3284, #18735 ) ;
#17473 = VECTOR ( 'NONE', #15375, 1000.000000000000000 ) ;
#17474 = ORIENTED_EDGE ( 'NONE', *, *, #18170, .F. ) ;
#17475 = PRODUCT_DEFINITION_SHAPE ( 'NONE', 'NONE',  #20376 ) ;
#17476 = ORIENTED_EDGE ( 'NONE', *, *, #1682, .F. ) ;
#17477 = CYLINDRICAL_SURFACE ( 'NONE', #700, 10.00000000000001066 ) ;
#17478 = CARTESIAN_POINT ( 'NONE',  ( -79.93116660809441498, 140.2969627923933729, 501.7130883271435096 ) ) ;
#17479 = ORIENTED_EDGE ( 'NONE', *, *, #9130, .T. ) ;
#17480 = ORIENTED_EDGE ( 'NONE', *, *, #3680, .T. ) ;
#17481 = DIRECTION ( 'NONE',  ( 1.000000000000000000, 0.000000000000000000, 0.000000000000000000 ) ) ;
#17482 =( LENGTH_UNIT ( ) NAMED_UNIT ( * ) SI_UNIT ( .MILLI., .METRE. ) );
#17483 =( NAMED_UNIT ( * ) PLANE_ANGLE_UNIT ( ) SI_UNIT ( $, .RADIAN. ) );
#17484 = DIRECTION ( 'NONE',  ( 0.000000000000000000, 0.000000000000000000, -1.000000000000000000 ) ) ;
#17485 = PLANE ( 'NONE',  #7837 ) ;
#17486 = DIRECTION ( 'NONE',  ( -0.000000000000000000, -1.000000000000000000, -0.000000000000000000 ) ) ;
#17487 = DIRECTION ( 'NONE',  ( -0.000000000000000000, -1.000000000000000000, -0.000000000000000000 ) ) ;
#17488 = DIRECTION ( 'NONE',  ( -0.000000000000000000, -0.000000000000000000, 1.000000000000000000 ) ) ;
#17489 = DIRECTION ( 'NONE',  ( -0.000000000000000000, 0.000000000000000000, 1.000000000000000000 ) ) ;
#17490 = DIRECTION ( 'NONE',  ( 1.000000000000000000, -0.000000000000000000, -0.000000000000000000 ) ) ;
#17491 = ORIENTED_EDGE ( 'NONE', *, *, #2283, .T. ) ;
#17492 = EDGE_CURVE ( 'NONE', #15883, #9757, #696, .T. ) ;
#17493 = VERTEX_POINT ( 'NONE', #10392 ) ;
#17494 = VECTOR ( 'NONE', #2077, 1000.000000000000000 ) ;
#17495 = VERTEX_POINT ( 'NONE', #1176 ) ;
#17496 = DIRECTION ( 'NONE',  ( 0.000000000000000000, -1.000000000000000000, 0.000000000000000000 ) ) ;
#17497 = ORIENTED_EDGE ( 'NONE', *, *, #5983, .F. ) ;
#17498 = ORIENTED_EDGE ( 'NONE', *, *, #12519, .F. ) ;
#17499 = CYLINDRICAL_SURFACE ( 'NONE', #1829, 9.500000000000000000 ) ;
#17500 = FILL_AREA_STYLE_COLOUR ( '', #18787 ) ;
#17501 = AXIS2_PLACEMENT_3D ( 'NONE', #2634, #7494, #7584 ) ;
#17502 = CARTESIAN_POINT ( 'NONE',  ( 7.000000000000000000, -17.52499999999999858, -2.146193515505736390E-15 ) ) ;
#17503 = CARTESIAN_POINT ( 'NONE',  ( 40.00000000000003553, 3.000000000000000000, 26.00000000000000355 ) ) ;
#17504 = SURFACE_STYLE_FILL_AREA ( #5266 ) ;
#17505 = LINE ( 'NONE', #3412, #13106 ) ;
#17506 = CIRCLE ( 'NONE', #5030, 0.9999999999999453770 ) ;
#17507 = VECTOR ( 'NONE', #8113, 1000.000000000000000 ) ;
#17508 = PLANE ( 'NONE',  #18560 ) ;
#17509 = EDGE_CURVE ( 'NONE', #17448, #18959, #19944, .T. ) ;
#17510 = CARTESIAN_POINT ( 'NONE',  ( 40.00000000000003553, 0.000000000000000000, -25.99999999999999645 ) ) ;
#17511 = FACE_OUTER_BOUND ( 'NONE', #14186, .T. ) ;
#17512 = VECTOR ( 'NONE', #20254, 1000.000000000000000 ) ;
#17513 = ORIENTED_EDGE ( 'NONE', *, *, #2069, .T. ) ;
#17514 = DIRECTION ( 'NONE',  ( -0.000000000000000000, -0.000000000000000000, 1.000000000000000000 ) ) ;
#17515 = CARTESIAN_POINT ( 'NONE',  ( 423.8334540492694487, 191.8198460455371333, 215.0057801310552179 ) ) ;
#17516 = PRODUCT_DEFINITION_FORMATION_WITH_SPECIFIED_SOURCE ( 'ANY', '', #17323, .NOT_KNOWN. ) ;
#17517 =( GEOMETRIC_REPRESENTATION_CONTEXT ( 3 ) GLOBAL_UNCERTAINTY_ASSIGNED_CONTEXT ( ( #9941 ) ) GLOBAL_UNIT_ASSIGNED_CONTEXT ( ( #353, #11394, #15071 ) ) REPRESENTATION_CONTEXT ( 'NONE', 'WORKASPACE' ) );
#17518 = VECTOR ( 'NONE', #13136, 1000.000000000000114 ) ;
#17519 = ORIENTED_EDGE ( 'NONE', *, *, #15093, .T. ) ;
#17520 = EDGE_CURVE ( 'NONE', #7477, #12937, #16883, .T. ) ;
#17521 = LINE ( 'NONE', #4969, #13010 ) ;
#17522 = VERTEX_POINT ( 'NONE', #2747 ) ;
#17523 = AXIS2_PLACEMENT_3D ( 'NONE', #17073, #3260, #17166 ) ;
#17524 = VECTOR ( 'NONE', #19836, 1000.000000000000000 ) ;
#17525 = CARTESIAN_POINT ( 'NONE',  ( 43.00000000000001421, 0.000000000000000000, -150.0000000000000000 ) ) ;
#17526 = ORIENTED_EDGE ( 'NONE', *, *, #2971, .T. ) ;
#17527 = DIRECTION ( 'NONE',  ( 0.000000000000000000, 0.000000000000000000, 1.000000000000000000 ) ) ;
#17528 = CARTESIAN_POINT ( 'NONE',  ( -40.00000000000000711, 0.000000000000000000, 26.00000000000000000 ) ) ;
#17529 = EDGE_LOOP ( 'NONE', ( #2548, #12628, #5186, #6838, #9424 ) ) ;
#17530 = CARTESIAN_POINT ( 'NONE',  ( -37.00000000000000711, 0.000000000000000000, 23.00000000000000000 ) ) ;
#17531 = DIRECTION ( 'NONE',  ( -0.000000000000000000, -1.000000000000000000, -0.000000000000000000 ) ) ;
#17532 = FACE_OUTER_BOUND ( 'NONE', #8348, .T. ) ;
#17533 =( GEOMETRIC_REPRESENTATION_CONTEXT ( 3 ) GLOBAL_UNCERTAINTY_ASSIGNED_CONTEXT ( ( #18316 ) ) GLOBAL_UNIT_ASSIGNED_CONTEXT ( ( #18525, #13709, #10500 ) ) REPRESENTATION_CONTEXT ( 'NONE', 'WORKASPACE' ) );
#17534 = EDGE_CURVE ( 'NONE', #18930, #10110, #5758, .T. ) ;
#17535 = CARTESIAN_POINT ( 'NONE',  ( 0.02524115952202954025, 140.1151673599038645, 501.4410921460604413 ) ) ;
#17536 = LINE ( 'NONE', #20323, #576 ) ;
#17537 = LINE ( 'NONE', #17849, #18099 ) ;
#17538 = CARTESIAN_POINT ( 'NONE',  ( 22.99999999999995737, 3.000000000000000000, -36.99999999999999289 ) ) ;
#17539 =( NAMED_UNIT ( * ) SI_UNIT ( $, .STERADIAN. ) SOLID_ANGLE_UNIT ( ) );
#17540 = VERTEX_POINT ( 'NONE', #20041 ) ;
#17541 = DIRECTION ( 'NONE',  ( -1.000000000000000000, 0.000000000000000000, 0.000000000000000000 ) ) ;
#17542 = ADVANCED_FACE ( 'NONE', ( #9043 ), #5945, .T. ) ;
#17543 = FACE_OUTER_BOUND ( 'NONE', #869, .T. ) ;
#17544 = AXIS2_PLACEMENT_3D ( 'NONE', #16524, #13522, #837 ) ;
#17545 = DIRECTION ( 'NONE',  ( -0.000000000000000000, -1.000000000000000000, -0.000000000000000000 ) ) ;
#17546 = PLANE ( 'NONE',  #12919 ) ;
#17547 = ORIENTED_EDGE ( 'NONE', *, *, #3216, .T. ) ;
#17548 = VERTEX_POINT ( 'NONE', #11192 ) ;
#17549 = EDGE_CURVE ( 'NONE', #3307, #15732, #17280, .T. ) ;
#17550 = PRESENTATION_LAYER_ASSIGNMENT (  '', '', ( #1407 ) ) ;
#17551 = AXIS2_PLACEMENT_3D ( 'NONE', #10685, #12045, #4210 ) ;
#17552 = ORIENTED_EDGE ( 'NONE', *, *, #18467, .T. ) ;
#17553 = ORIENTED_EDGE ( 'NONE', *, *, #324, .T. ) ;
#17554 = DIRECTION ( 'NONE',  ( 0.000000000000000000, 0.000000000000000000, -1.000000000000000000 ) ) ;
#17555 = EDGE_CURVE ( 'NONE', #15498, #6182, #3262, .T. ) ;
#17556 = ORIENTED_EDGE ( 'NONE', *, *, #8146, .T. ) ;
#17557 = AXIS2_PLACEMENT_3D ( 'NONE', #5446, #4295, #13571 ) ;
#17558 = FACE_BOUND ( 'NONE', #3951, .T. ) ;
#17559 = DIRECTION ( 'NONE',  ( -1.000000000000000000, -0.000000000000000000, -0.000000000000000000 ) ) ;
#17560 = ORIENTED_EDGE ( 'NONE', *, *, #10033, .T. ) ;
#17561 = EDGE_CURVE ( 'NONE', #19713, #13515, #15129, .T. ) ;
#17562 = CARTESIAN_POINT ( 'NONE',  ( -211.5106270998635409, 123.1299228374912644, 79.58252780074349175 ) ) ;
#17563 = SURFACE_STYLE_FILL_AREA ( #11276 ) ;
#17564 = FILL_AREA_STYLE ('',( #14381 ) ) ;
#17565 = CARTESIAN_POINT ( 'NONE',  ( -211.5106270998635409, 103.1299228374912360, 170.4174721992565082 ) ) ;
#17566 = LINE ( 'NONE', #354, #10048 ) ;
#17567 = FACE_OUTER_BOUND ( 'NONE', #20164, .T. ) ;
#17568 = VECTOR ( 'NONE', #6128, 1000.000000000000000 ) ;
#17569 = LINE ( 'NONE', #12851, #18232 ) ;
#17570 = VECTOR ( 'NONE', #697, 1000.000000000000000 ) ;
#17571 = EDGE_LOOP ( 'NONE', ( #13076, #557, #3859, #9645, #16886, #6630, #19089, #9883 ) ) ;
#17572 = CARTESIAN_POINT ( 'NONE',  ( 4.025000000000000355, 0.000000000000000000, 0.000000000000000000 ) ) ;
#17573 = ADVANCED_FACE ( 'NONE', ( #9234 ), #11095, .F. ) ;
#17574 =( NAMED_UNIT ( * ) PLANE_ANGLE_UNIT ( ) SI_UNIT ( $, .RADIAN. ) );
#17575 = SURFACE_STYLE_FILL_AREA ( #9849 ) ;
#17576 = DIRECTION ( 'NONE',  ( -1.000000000000000000, -0.000000000000000000, -3.328238341717372086E-14 ) ) ;
#17577 =( LENGTH_UNIT ( ) NAMED_UNIT ( * ) SI_UNIT ( .MILLI., .METRE. ) );
#17578 = CARTESIAN_POINT ( 'NONE',  ( 406.3334540492693350, 242.8734308960556234, 0.000000000000000000 ) ) ;
#17579 = FILL_AREA_STYLE_COLOUR ( '', #5592 ) ;
#17580 = AXIS2_PLACEMENT_3D ( 'NONE', #15429, #18909, #3160 ) ;
#17581 = EDGE_LOOP ( 'NONE', ( #9014, #18487, #18009, #5193 ) ) ;
#17582 = VECTOR ( 'NONE', #15079, 1000.000000000000114 ) ;
#17583 = COLOUR_RGB ( '', 0.09019608, 0.27058824, 0.51372549) ;
#17584 = EDGE_CURVE ( 'NONE', #19713, #7546, #12568, .T. ) ;
#17585 = EDGE_LOOP ( 'NONE', ( #16940, #5883, #2761, #13081 ) ) ;
#17586 = ORIENTED_EDGE ( 'NONE', *, *, #6131, .F. ) ;
#17587 = VECTOR ( 'NONE', #7626, 1000.000000000000000 ) ;
#17588 = AXIS2_PLACEMENT_3D ( 'NONE', #179, #14399, #6376 ) ;
#17589 = VERTEX_POINT ( 'NONE', #20353 ) ;
#17590 = CARTESIAN_POINT ( 'NONE',  ( 20.99999999999996092, -20.00000000000000000, 35.00000000000000711 ) ) ;
#17591 = CARTESIAN_POINT ( 'NONE',  ( -80.17038797525196969, 140.8458045485498360, 501.2617728964195862 ) ) ;
#17592 = VECTOR ( 'NONE', #9104, 1000.000000000000000 ) ;
#17593 = ORIENTED_EDGE ( 'NONE', *, *, #12438, .F. ) ;
#17594 = CYLINDRICAL_SURFACE ( 'NONE', #5101, 10.00000000000000888 ) ;
#17595 = LINE ( 'NONE', #8329, #389 ) ;
#17596 = EDGE_LOOP ( 'NONE', ( #7505, #459 ) ) ;
#17597 = EDGE_CURVE ( 'NONE', #19312, #10280, #1686, .T. ) ;
#17598 = VECTOR ( 'NONE', #11157, 1000.000000000000000 ) ;
#17599 = VECTOR ( 'NONE', #12491, 1000.000000000000000 ) ;
#17600 = CARTESIAN_POINT ( 'NONE',  ( -211.5106270998635409, 123.1299228374912644, 29.36128450348865471 ) ) ;
#17601 = AXIS2_PLACEMENT_3D ( 'NONE', #12988, #14721, #10084 ) ;
#17602 = DIRECTION ( 'NONE',  ( 0.000000000000000000, -1.000000000000000000, 0.000000000000000000 ) ) ;
#17603 = LINE ( 'NONE', #9459, #5439 ) ;
#17604 = VECTOR ( 'NONE', #20069, 1000.000000000000000 ) ;
#17605 = EDGE_CURVE ( 'NONE', #17151, #4707, #10790, .T. ) ;
#17606 = CARTESIAN_POINT ( 'NONE',  ( 153.4893729001366864, 113.1299228374914634, 170.4174721992565082 ) ) ;
#17607 = EDGE_CURVE ( 'NONE', #5330, #11362, #18801, .T. ) ;
#17608 = CARTESIAN_POINT ( 'NONE',  ( 8.420862748423350279E-16, 6.000000000000000000, 12.50000000000000000 ) ) ;
#17609 =( LENGTH_UNIT ( ) NAMED_UNIT ( * ) SI_UNIT ( .MILLI., .METRE. ) );
#17610 = DIRECTION ( 'NONE',  ( 0.000000000000000000, 1.000000000000000000, 0.000000000000000000 ) ) ;
#17611 = MECHANICAL_DESIGN_GEOMETRIC_PRESENTATION_REPRESENTATION (  '', ( #14649 ), #10692 ) ;
#17612 = CARTESIAN_POINT ( 'NONE',  ( -23.00000000000003197, 0.000000000000000000, 34.00000000000000711 ) ) ;
#17613 = PRESENTATION_LAYER_ASSIGNMENT (  '', '', ( #18919 ) ) ;
#17614 = LINE ( 'NONE', #17396, #12206 ) ;
#17615 = EDGE_LOOP ( 'NONE', ( #2713, #3294, #8036, #1084 ) ) ;
#17616 = AXIS2_PLACEMENT_3D ( 'NONE', #18521, #15248, #4418 ) ;
#17617 = ORIENTED_EDGE ( 'NONE', *, *, #19444, .T. ) ;
#17618 = ORIENTED_EDGE ( 'NONE', *, *, #19234, .F. ) ;
#17619 = UNCERTAINTY_MEASURE_WITH_UNIT (LENGTH_MEASURE( 1.000000000000000082E-05 ), #3816, 'distance_accuracy_value', 'NONE');
#17620 = CIRCLE ( 'NONE', #7733, 8.000000000000007105 ) ;
#17621 = CARTESIAN_POINT ( 'NONE',  ( -31.00000000000005329, 0.000000000000000000, 26.00000000000000000 ) ) ;
#17622 = VERTEX_POINT ( 'NONE', #8601 ) ;
#17623 = VERTEX_POINT ( 'NONE', #19415 ) ;
#17624 = ORIENTED_EDGE ( 'NONE', *, *, #5701, .F. ) ;
#17625 = DIRECTION ( 'NONE',  ( 0.000000000000000000, 1.000000000000000000, 0.000000000000000000 ) ) ;
#17626 = CARTESIAN_POINT ( 'NONE',  ( 463.8334540492693350, 214.2156642432025251, 0.000000000000000000 ) ) ;
#17627 = CARTESIAN_POINT ( 'NONE',  ( 21.99999999999998224, 6.000000000000000000, -31.99999999999998579 ) ) ;
#17628 = COLOUR_RGB ( '', 0.40784314, 0.44705882, 0.49803922) ;
#17629 = DIRECTION ( 'NONE',  ( 0.000000000000000000, 0.000000000000000000, -1.000000000000000000 ) ) ;
#17630 = EDGE_CURVE ( 'NONE', #18105, #7143, #4344, .T. ) ;
#17631 = DIRECTION ( 'NONE',  ( -0.000000000000000000, -1.000000000000000000, -0.000000000000000000 ) ) ;
#17632 = DIRECTION ( 'NONE',  ( 1.000000000000000000, 0.000000000000000000, 3.328238341717372086E-14 ) ) ;
#17633 = APPLICATION_CONTEXT ( 'automotive_design' ) ;
#17634 = FACE_OUTER_BOUND ( 'NONE', #16808, .T. ) ;
#17635 =( LENGTH_UNIT ( ) NAMED_UNIT ( * ) SI_UNIT ( .MILLI., .METRE. ) );
#17636 = LINE ( 'NONE', #14229, #4088 ) ;
#17637 = DIRECTION ( 'NONE',  ( -0.000000000000000000, -1.000000000000000000, 0.000000000000000000 ) ) ;
#17638 = CIRCLE ( 'NONE', #6467, 5.000000000000000888 ) ;
#17639 = ORIENTED_EDGE ( 'NONE', *, *, #13533, .T. ) ;
#17640 = CARTESIAN_POINT ( 'NONE',  ( 111.4893729001366012, 127.7247684487574304, 252.0000000000000000 ) ) ;
#17641 = ORIENTED_EDGE ( 'NONE', *, *, #17095, .F. ) ;
#17642 =( NAMED_UNIT ( * ) SI_UNIT ( $, .STERADIAN. ) SOLID_ANGLE_UNIT ( ) );
#17643 = ORIENTED_EDGE ( 'NONE', *, *, #19714, .T. ) ;
#17644 = DIRECTION ( 'NONE',  ( -0.000000000000000000, -1.000000000000000000, -0.000000000000000000 ) ) ;
#17645 = DIRECTION ( 'NONE',  ( -0.000000000000000000, -1.000000000000000000, -1.632680918566406547E-16 ) ) ;
#17646 = ORIENTED_EDGE ( 'NONE', *, *, #2947, .T. ) ;
#17647 = CARTESIAN_POINT ( 'NONE',  ( -25.99999999999999645, 0.000000000000000000, 40.00000000000002132 ) ) ;
#17648 = FILL_AREA_STYLE ('',( #16229 ) ) ;
#17649 = VECTOR ( 'NONE', #5870, 1000.000000000000000 ) ;
#17650 = ADVANCED_FACE ( 'NONE', ( #19323 ), #663, .T. ) ;
#17651 = PRESENTATION_STYLE_ASSIGNMENT (( #11366 ) ) ;
#17652 = VECTOR ( 'NONE', #10588, 1000.000000000000000 ) ;
#17653 = SURFACE_SIDE_STYLE ('',( #8282 ) ) ;
#17654 = PLANE ( 'NONE',  #20150 ) ;
#17655 = FACE_OUTER_BOUND ( 'NONE', #19059, .T. ) ;
#17656 = PRESENTATION_STYLE_ASSIGNMENT (( #6757 ) ) ;
#17657 = ORIENTED_EDGE ( 'NONE', *, *, #18645, .T. ) ;
#17658 = SURFACE_STYLE_USAGE ( .BOTH. , #5398 ) ;
#17659 = LINE ( 'NONE', #3546, #10224 ) ;
#17660 = DIRECTION ( 'NONE',  ( 1.000000000000000000, 0.000000000000000000, 0.000000000000000000 ) ) ;
#17661 = ITEM_DEFINED_TRANSFORMATION ( 'NONE', 'NONE', #6678,  #2741 ) ;
#17662 = PRODUCT ( 'Part14', 'Part14', '', ( #4188 ) ) ;
#17663 = ORIENTED_EDGE ( 'NONE', *, *, #11033, .T. ) ;
#17664 = FACE_OUTER_BOUND ( 'NONE', #10720, .T. ) ;
#17665 = EDGE_LOOP ( 'NONE', ( #16323, #12235, #13560, #3584 ) ) ;
#17666 = EDGE_LOOP ( 'NONE', ( #5164, #1900, #7829, #6267 ) ) ;
#17667 = EDGE_CURVE ( 'NONE', #298, #18105, #3878, .T. ) ;
#17668 = VERTEX_POINT ( 'NONE', #14895 ) ;
#17669 = AXIS2_PLACEMENT_3D ( 'NONE', #2119, #8435, #13175 ) ;
#17670 = LINE ( 'NONE', #13147, #9742 ) ;
#17671 = EDGE_LOOP ( 'NONE', ( #15693, #16559 ) ) ;
#17672 = CARTESIAN_POINT ( 'NONE',  ( 0.3607327643218288804, 139.8077789474102133, 489.3460758413267513 ) ) ;
#17673 = ORIENTED_EDGE ( 'NONE', *, *, #15828, .F. ) ;
#17674 = LINE ( 'NONE', #14776, #2137 ) ;
#17675 = CARTESIAN_POINT ( 'NONE',  ( 463.8334540492693350, 191.8198460455371333, 14.99421986894475012 ) ) ;
#17676 = CARTESIAN_POINT ( 'NONE',  ( 78.48937290013660117, 145.9162550801369491, -97.94896630388704750 ) ) ;
#17677 = DIRECTION ( 'NONE',  ( -0.000000000000000000, -0.000000000000000000, -1.000000000000000000 ) ) ;
#17678 = DIRECTION ( 'NONE',  ( -0.000000000000000000, -1.000000000000000000, -0.000000000000000000 ) ) ;
#17679 = EDGE_CURVE ( 'NONE', #6521, #4192, #11291, .T. ) ;
#17680 = DIRECTION ( 'NONE',  ( 0.000000000000000000, 0.000000000000000000, 1.000000000000000000 ) ) ;
#17681 = ORIENTED_EDGE ( 'NONE', *, *, #9691, .T. ) ;
#17682 = DIRECTION ( 'NONE',  ( 0.000000000000000000, 1.000000000000000000, 7.137148015447440312E-15 ) ) ;
#17683 = CARTESIAN_POINT ( 'NONE',  ( 111.4893729001365870, 209.1356689931817812, 347.4957642363283412 ) ) ;
#17684 = CARTESIAN_POINT ( 'NONE',  ( 153.4893729001366864, 103.1299228374914492, 79.58252780074349175 ) ) ;
#17685 =( LENGTH_UNIT ( ) NAMED_UNIT ( * ) SI_UNIT ( .MILLI., .METRE. ) );
#17686 = EDGE_CURVE ( 'NONE', #5571, #10263, #16171, .T. ) ;
#17687 = DIRECTION ( 'NONE',  ( 1.000000000000000000, 0.000000000000000000, 0.000000000000000000 ) ) ;
#17688 = ORIENTED_EDGE ( 'NONE', *, *, #7017, .T. ) ;
#17689 = ORIENTED_EDGE ( 'NONE', *, *, #2109, .T. ) ;
#17690 = EDGE_CURVE ( 'NONE', #19061, #4894, #11718, .T. ) ;
#17691 = CIRCLE ( 'NONE', #18984, 3.000000000000002665 ) ;
#17692 = EDGE_LOOP ( 'NONE', ( #4580, #11765, #8517, #14187 ) ) ;
#17693 = EDGE_CURVE ( 'NONE', #10110, #17281, #19131, .T. ) ;
#17694 = CARTESIAN_POINT ( 'NONE',  ( -79.99999999999995737, 141.4538982823126503, 501.7130837607361968 ) ) ;
#17695 = ORIENTED_EDGE ( 'NONE', *, *, #9900, .T. ) ;
#17696 = DIRECTION ( 'NONE',  ( 1.000000000000000000, 1.197852309262419498E-15, -0.000000000000000000 ) ) ;
#17697 = FILL_AREA_STYLE_COLOUR ( '', #2700 ) ;
#17698 = ORIENTED_EDGE ( 'NONE', *, *, #13866, .F. ) ;
#17699 = DIRECTION ( 'NONE',  ( -0.000000000000000000, -1.000000000000000000, -0.000000000000000000 ) ) ;
#17700 = CARTESIAN_POINT ( 'NONE',  ( 53.48937290013658696, 126.1646452518344859, 280.0825295754780768 ) ) ;
#17701 = FACE_BOUND ( 'NONE', #13054, .T. ) ;
#17702 = EDGE_CURVE ( 'NONE', #14088, #9458, #8424, .T. ) ;
#17703 = CARTESIAN_POINT ( 'NONE',  ( 498.8334540492693918, 167.8734308960555950, 0.000000000000000000 ) ) ;
#17704 = CARTESIAN_POINT ( 'NONE',  ( 0.000000000000000000, 0.000000000000000000, 0.000000000000000000 ) ) ;
#17705 = LINE ( 'NONE', #11521, #15655 ) ;
#17706 = DIRECTION ( 'NONE',  ( -0.000000000000000000, -1.000000000000000000, -0.000000000000000000 ) ) ;
#17707 = DIRECTION ( 'NONE',  ( 1.000000000000000000, 2.135044278125300850E-16, -0.000000000000000000 ) ) ;
#17708 = VECTOR ( 'NONE', #15539, 1000.000000000000000 ) ;
#17709 =( NAMED_UNIT ( * ) SI_UNIT ( $, .STERADIAN. ) SOLID_ANGLE_UNIT ( ) );
#17710 = ORIENTED_EDGE ( 'NONE', *, *, #5973, .T. ) ;
#17711 = EDGE_CURVE ( 'NONE', #15663, #15103, #15867, .T. ) ;
#17712 = EDGE_LOOP ( 'NONE', ( #12863, #15781, #3703, #11405, #1074 ) ) ;
#17713 = EDGE_CURVE ( 'NONE', #13911, #17228, #6974, .T. ) ;
#17714 = ORIENTED_EDGE ( 'NONE', *, *, #2312, .T. ) ;
#17715 = ORIENTED_EDGE ( 'NONE', *, *, #4845, .F. ) ;
#17716 = ORIENTED_EDGE ( 'NONE', *, *, #843, .T. ) ;
#17717 = DIRECTION ( 'NONE',  ( 1.000000000000000000, 0.000000000000000000, 0.000000000000000000 ) ) ;
#17718 = CARTESIAN_POINT ( 'NONE',  ( 4.286263797015737285E-15, -3.000000000000000000, -35.00000000000000711 ) ) ;
#17719 = AXIS2_PLACEMENT_3D ( 'NONE', #8594, #17777, #13373 ) ;
#17720 = CARTESIAN_POINT ( 'NONE',  ( -40.00000000000000711, 10.00000000000000000, -19.00000000000000355 ) ) ;
#17721 = CARTESIAN_POINT ( 'NONE',  ( -81.18192946989242387, 139.7703989349477354, 490.5655098180907885 ) ) ;
#17722 = DIRECTION ( 'NONE',  ( 0.000000000000000000, 1.000000000000000000, 0.000000000000000000 ) ) ;
#17723 = DIRECTION ( 'NONE',  ( 0.000000000000000000, 1.000000000000000000, 0.000000000000000000 ) ) ;
#17724 = CARTESIAN_POINT ( 'NONE',  ( 2.844582250340499385, 60.97290968073905759, 9.064464814046607088 ) ) ;
#17725 = PLANE ( 'NONE',  #8470 ) ;
#17726 = FILL_AREA_STYLE ('',( #19362 ) ) ;
#17727 = LINE ( 'NONE', #13211, #18765 ) ;
#17728 =( NAMED_UNIT ( * ) SI_UNIT ( $, .STERADIAN. ) SOLID_ANGLE_UNIT ( ) );
#17729 = ADVANCED_FACE ( 'NONE', ( #1997 ), #19116, .F. ) ;
#17730 = DIRECTION ( 'NONE',  ( 0.000000000000000000, 0.000000000000000000, 1.000000000000000000 ) ) ;
#17731 = CARTESIAN_POINT ( 'NONE',  ( -75.00000000000000000, 313.8311070602663904, -142.2176018917206761 ) ) ;
#17732 =( GEOMETRIC_REPRESENTATION_CONTEXT ( 3 ) GLOBAL_UNCERTAINTY_ASSIGNED_CONTEXT ( ( #19400 ) ) GLOBAL_UNIT_ASSIGNED_CONTEXT ( ( #10454, #13952, #945 ) ) REPRESENTATION_CONTEXT ( 'NONE', 'WORKASPACE' ) );
#17733 = EDGE_CURVE ( 'NONE', #15663, #17495, #3575, .T. ) ;
#17734 = ORIENTED_EDGE ( 'NONE', *, *, #3732, .T. ) ;
#17735 = DIRECTION ( 'NONE',  ( -1.000000000000000000, 0.000000000000000000, 0.000000000000000000 ) ) ;
#17736 = UNCERTAINTY_MEASURE_WITH_UNIT (LENGTH_MEASURE( 1.000000000000000082E-05 ), #637, 'distance_accuracy_value', 'NONE');
#17737 = EDGE_LOOP ( 'NONE', ( #1823, #1570 ) ) ;
#17738 = CARTESIAN_POINT ( 'NONE',  ( -30.99999999999999645, 0.000000000000000000, -30.99999999999999289 ) ) ;
#17739 = ORIENTED_EDGE ( 'NONE', *, *, #19357, .F. ) ;
#17740 = UNCERTAINTY_MEASURE_WITH_UNIT (LENGTH_MEASURE( 1.000000000000000082E-05 ), #6357, 'distance_accuracy_value', 'NONE');
#17741 =( NAMED_UNIT ( * ) PLANE_ANGLE_UNIT ( ) SI_UNIT ( $, .RADIAN. ) );
#17742 = DIRECTION ( 'NONE',  ( 1.000000000000000000, 5.889072920838430686E-16, -0.000000000000000000 ) ) ;
#17743 = UNCERTAINTY_MEASURE_WITH_UNIT (LENGTH_MEASURE( 1.000000000000000082E-05 ), #2162, 'distance_accuracy_value', 'NONE');
#17744 = ORIENTED_EDGE ( 'NONE', *, *, #10751, .F. ) ;
#17745 = CARTESIAN_POINT ( 'NONE',  ( 10.00000000000000000, 372.8685141053778693, -86.48019484660871115 ) ) ;
#17746 = CIRCLE ( 'NONE', #1290, 17.52499999999999858 ) ;
#17747 =( LENGTH_UNIT ( ) NAMED_UNIT ( * ) SI_UNIT ( .MILLI., .METRE. ) );
#17748 = CARTESIAN_POINT ( 'NONE',  ( -78.99999999999995737, 146.8256012863087676, 480.6843163258853906 ) ) ;
#17749 = CIRCLE ( 'NONE', #12817, 3.299999999999997158 ) ;
#17750 = LINE ( 'NONE', #10126, #18872 ) ;
#17751 = SURFACE_SIDE_STYLE ('',( #5197 ) ) ;
#17752 = DIRECTION ( 'NONE',  ( 0.000000000000000000, 0.000000000000000000, -1.000000000000000000 ) ) ;
#17753 = ORIENTED_EDGE ( 'NONE', *, *, #4766, .T. ) ;
#17754 = DIRECTION ( 'NONE',  ( 0.000000000000000000, 0.000000000000000000, 1.000000000000000000 ) ) ;
#17755 = DIRECTION ( 'NONE',  ( -0.000000000000000000, 1.000000000000000000, -0.000000000000000000 ) ) ;
#17756 = DIRECTION ( 'NONE',  ( 0.000000000000000000, 0.000000000000000000, -1.000000000000000000 ) ) ;
#17757 = LINE ( 'NONE', #16046, #1344 ) ;
#17758 = ORIENTED_EDGE ( 'NONE', *, *, #18804, .T. ) ;
#17759 =( GEOMETRIC_REPRESENTATION_CONTEXT ( 3 ) GLOBAL_UNCERTAINTY_ASSIGNED_CONTEXT ( ( #8665 ) ) GLOBAL_UNIT_ASSIGNED_CONTEXT ( ( #5784, #9074, #16718 ) ) REPRESENTATION_CONTEXT ( 'NONE', 'WORKASPACE' ) );
#17760 = VECTOR ( 'NONE', #8763, 1000.000000000000000 ) ;
#17761 = ADVANCED_FACE ( 'NONE', ( #13167 ), #11601, .T. ) ;
#17762 = VERTEX_POINT ( 'NONE', #16855 ) ;
#17763 = VERTEX_POINT ( 'NONE', #18377 ) ;
#17764 = FACE_BOUND ( 'NONE', #14018, .T. ) ;
#17765 = UNCERTAINTY_MEASURE_WITH_UNIT (LENGTH_MEASURE( 1.000000000000000082E-05 ), #10329, 'distance_accuracy_value', 'NONE');
#17766 = LINE ( 'NONE', #17970, #18867 ) ;
#17767 = LINE ( 'NONE', #14876, #8645 ) ;
#17768 = ORIENTED_EDGE ( 'NONE', *, *, #15801, .T. ) ;
#17769 = FILL_AREA_STYLE_COLOUR ( '', #1047 ) ;
#17770 = VECTOR ( 'NONE', #12341, 1000.000000000000000 ) ;
#17771 = CARTESIAN_POINT ( 'NONE',  ( 40.00000000000000711, 11.00000000000000000, -26.00000000000000355 ) ) ;
#17772 = VECTOR ( 'NONE', #3686, 1000.000000000000000 ) ;
#17773 = PLANE ( 'NONE',  #6241 ) ;
#17774 = CIRCLE ( 'NONE', #20047, 1.000000000000000000 ) ;
#17775 = DIRECTION ( 'NONE',  ( 0.000000000000000000, 0.000000000000000000, 1.000000000000000000 ) ) ;
#17776 = EDGE_LOOP ( 'NONE', ( #14192, #16440, #14134, #830 ) ) ;
#17777 = DIRECTION ( 'NONE',  ( 1.000000000000000000, 0.000000000000000000, 0.000000000000000000 ) ) ;
#17778 = SURFACE_STYLE_FILL_AREA ( #11713 ) ;
#17779 = SURFACE_SIDE_STYLE ('',( #261 ) ) ;
#17780 = DIRECTION ( 'NONE',  ( 0.000000000000000000, -0.000000000000000000, 1.000000000000000000 ) ) ;
#17781 = CARTESIAN_POINT ( 'NONE',  ( 55.48937290013659407, 209.7811923590224978, 348.0151256184570343 ) ) ;
#17782 = EDGE_LOOP ( 'NONE', ( #14350, #16961, #11234, #18432, #17480 ) ) ;
#17783 = ORIENTED_EDGE ( 'NONE', *, *, #16462, .F. ) ;
#17784 = AXIS2_PLACEMENT_3D ( 'NONE', #4897, #10591, #20052 ) ;
#17785 = VECTOR ( 'NONE', #17955, 1000.000000000000000 ) ;
#17786 = ADVANCED_FACE ( 'NONE', ( #4079 ), #12022, .F. ) ;
#17787 = ORIENTED_EDGE ( 'NONE', *, *, #9777, .T. ) ;
#17788 = DIRECTION ( 'NONE',  ( 0.000000000000000000, 0.000000000000000000, -1.000000000000000000 ) ) ;
#17789 = CARTESIAN_POINT ( 'NONE',  ( -21.00000000000002842, 3.000000000000000000, -37.50000000000000000 ) ) ;
#17790 = ORIENTED_EDGE ( 'NONE', *, *, #4348, .T. ) ;
#17791 =( NAMED_UNIT ( * ) SI_UNIT ( $, .STERADIAN. ) SOLID_ANGLE_UNIT ( ) );
#17792 = EDGE_CURVE ( 'NONE', #15525, #19679, #3362, .T. ) ;
#17793 = CIRCLE ( 'NONE', #15526, 3.000000000000000888 ) ;
#17794 = VERTEX_POINT ( 'NONE', #15413 ) ;
#17795 = CARTESIAN_POINT ( 'NONE',  ( 31.00000000000003553, 10.00000000000000000, -22.99999999999999645 ) ) ;
#17796 = CARTESIAN_POINT ( 'NONE',  ( -34.99999999999996447, 8.000000000000000000, 40.00000000000000711 ) ) ;
#17797 = CARTESIAN_POINT ( 'NONE',  ( -0.2419462974620343876, 138.8109269117517499, 490.0408395169303617 ) ) ;
#17798 = DIRECTION ( 'NONE',  ( -0.000000000000000000, -1.000000000000000000, -0.000000000000000000 ) ) ;
#17799 = AXIS2_PLACEMENT_3D ( 'NONE', #7669, #18588, #6331 ) ;
#17800 = DIRECTION ( 'NONE',  ( -0.000000000000000000, -1.000000000000000000, -0.000000000000000000 ) ) ;
#17801 = COLOUR_RGB ( '', 0.66274510, 0.83137255, 0.94901961) ;
#17802 = DIRECTION ( 'NONE',  ( 0.000000000000000000, 1.000000000000000000, 0.000000000000000000 ) ) ;
#17803 = CARTESIAN_POINT ( 'NONE',  ( -31.00000000000002132, 10.00000000000000000, -31.00000000000000000 ) ) ;
#17804 = ORIENTED_EDGE ( 'NONE', *, *, #7976, .F. ) ;
#17805 = FACE_OUTER_BOUND ( 'NONE', #17615, .T. ) ;
#17806 = SURFACE_SIDE_STYLE ('',( #8448 ) ) ;
#17807 = ADVANCED_FACE ( 'NONE', ( #11913 ), #15102, .T. ) ;
#17808 = VERTEX_POINT ( 'NONE', #3972 ) ;
#17809 = ORIENTED_EDGE ( 'NONE', *, *, #11697, .T. ) ;
#17810 = EDGE_CURVE ( 'NONE', #4175, #9239, #10461, .T. ) ;
#17811 = VERTEX_POINT ( 'NONE', #19921 ) ;
#17812 = ORIENTED_EDGE ( 'NONE', *, *, #10679, .T. ) ;
#17813 = SURFACE_STYLE_USAGE ( .BOTH. , #5462 ) ;
#17814 =( GEOMETRIC_REPRESENTATION_CONTEXT ( 3 ) GLOBAL_UNCERTAINTY_ASSIGNED_CONTEXT ( ( #2880 ) ) GLOBAL_UNIT_ASSIGNED_CONTEXT ( ( #3697, #2229, #17709 ) ) REPRESENTATION_CONTEXT ( 'NONE', 'WORKASPACE' ) );
#17815 = LINE ( 'NONE', #16202, #2419 ) ;
#17816 = ADVANCED_FACE ( 'NONE', ( #2523 ), #19616, .T. ) ;
#17817 = CARTESIAN_POINT ( 'NONE',  ( 2.799999999999999822, 13.30000000000000071, 0.000000000000000000 ) ) ;
#17818 = ADVANCED_FACE ( 'NONE', ( #15521 ), #6445, .F. ) ;
#17819 = DIRECTION ( 'NONE',  ( -1.000000000000000000, 0.000000000000000000, 0.000000000000000000 ) ) ;
#17820 = DIRECTION ( 'NONE',  ( -0.000000000000000000, -0.000000000000000000, 1.000000000000000000 ) ) ;
#17821 = CARTESIAN_POINT ( 'NONE',  ( -79.99999999999995737, 216.7545334744432921, 495.1946179577816451 ) ) ;
#17822 = DIRECTION ( 'NONE',  ( 1.000000000000000000, -0.000000000000000000, 0.000000000000000000 ) ) ;
#17823 = EDGE_CURVE ( 'NONE', #18834, #16767, #7009, .T. ) ;
#17824 = DIRECTION ( 'NONE',  ( 0.000000000000000000, -0.000000000000000000, -1.000000000000000000 ) ) ;
#17825 = DIRECTION ( 'NONE',  ( 0.000000000000000000, 1.000000000000000000, 0.000000000000000000 ) ) ;
#17826 = EDGE_CURVE ( 'NONE', #6561, #14242, #11073, .T. ) ;
#17827 = CARTESIAN_POINT ( 'NONE',  ( 78.48937290013660117, 113.1299228374914208, 220.6387154965113382 ) ) ;
#17828 = CARTESIAN_POINT ( 'NONE',  ( 111.4893729001366154, 77.72476844875745883, 250.0000000000000000 ) ) ;
#17829 = AXIS2_PLACEMENT_3D ( 'NONE', #572, #10064, #8213 ) ;
#17830 = AXIS2_PLACEMENT_3D ( 'NONE', #12658, #8012, #12349 ) ;
#17831 = ORIENTED_EDGE ( 'NONE', *, *, #15665, .T. ) ;
#17832 = FACE_OUTER_BOUND ( 'NONE', #2524, .T. ) ;
#17833 = ORIENTED_EDGE ( 'NONE', *, *, #18807, .F. ) ;
#17834 = ORIENTED_EDGE ( 'NONE', *, *, #6765, .T. ) ;
#17835 = LINE ( 'NONE', #2370, #20081 ) ;
#17836 = ORIENTED_EDGE ( 'NONE', *, *, #12446, .T. ) ;
#17837 = LINE ( 'NONE', #8473, #7728 ) ;
#17838 = AXIS2_PLACEMENT_3D ( 'NONE', #11210, #3390, #10919 ) ;
#17839 =( GEOMETRIC_REPRESENTATION_CONTEXT ( 3 ) GLOBAL_UNCERTAINTY_ASSIGNED_CONTEXT ( ( #1208 ) ) GLOBAL_UNIT_ASSIGNED_CONTEXT ( ( #12422, #9423, #6144 ) ) REPRESENTATION_CONTEXT ( 'NONE', 'WORKASPACE' ) );
#17840 = DIRECTION ( 'NONE',  ( -1.000000000000000000, 0.000000000000000000, -1.734723475976807094E-15 ) ) ;
#17841 = ORIENTED_EDGE ( 'NONE', *, *, #3173, .T. ) ;
#17842 = DIRECTION ( 'NONE',  ( -0.000000000000000000, -0.000000000000000000, 1.000000000000000000 ) ) ;
#17843 = DIRECTION ( 'NONE',  ( 0.000000000000000000, 0.000000000000000000, -1.000000000000000000 ) ) ;
#17844 = FACE_OUTER_BOUND ( 'NONE', #18778, .T. ) ;
#17845 = MECHANICAL_DESIGN_GEOMETRIC_PRESENTATION_REPRESENTATION (  '', ( #71 ), #18482 ) ;
#17846 = EDGE_CURVE ( 'NONE', #9405, #15351, #13961, .T. ) ;
#17847 = DIRECTION ( 'NONE',  ( 1.000000000000000000, 5.889072920838430686E-16, -0.000000000000000000 ) ) ;
#17848 = FACE_OUTER_BOUND ( 'NONE', #16626, .T. ) ;
#17849 = CARTESIAN_POINT ( 'NONE',  ( 20.99999999999996092, -20.00000000000000000, 32.50000000000000711 ) ) ;
#17850 = PRODUCT_DEFINITION_FORMATION_WITH_SPECIFIED_SOURCE ( 'ANY', '', #3169, .NOT_KNOWN. ) ;
#17851 = DIRECTION ( 'NONE',  ( 0.000000000000000000, -1.000000000000000000, 0.000000000000000000 ) ) ;
#17852 = EDGE_CURVE ( 'NONE', #4170, #18513, #4485, .T. ) ;
#17853 = ORIENTED_EDGE ( 'NONE', *, *, #19145, .T. ) ;
#17854 = CARTESIAN_POINT ( 'NONE',  ( -211.5106270998635409, 113.1299228374912502, 79.58252780074349175 ) ) ;
#17855 = VECTOR ( 'NONE', #9821, 1000.000000000000000 ) ;
#17856 = CARTESIAN_POINT ( 'NONE',  ( 23.00000000000000711, 0.000000000000000000, -31.00000000000002487 ) ) ;
#17857 = ADVANCED_FACE ( 'NONE', ( #10765 ), #13569, .T. ) ;
#17858 = ORIENTED_EDGE ( 'NONE', *, *, #92, .T. ) ;
#17859 = VECTOR ( 'NONE', #430, 1000.000000000000000 ) ;
#17860 = AXIS2_PLACEMENT_3D ( 'NONE', #17870, #19220, #8497 ) ;
#17861 = ORIENTED_EDGE ( 'NONE', *, *, #1540, .F. ) ;
#17862 = VERTEX_POINT ( 'NONE', #12304 ) ;
#17863 = DIRECTION ( 'NONE',  ( 1.000000000000000000, -0.000000000000000000, 0.000000000000000000 ) ) ;
#17864 = PRODUCT_DEFINITION_FORMATION_WITH_SPECIFIED_SOURCE ( 'ANY', '', #7941, .NOT_KNOWN. ) ;
#17865 = ORIENTED_EDGE ( 'NONE', *, *, #5695, .F. ) ;
#17866 = SURFACE_STYLE_USAGE ( .BOTH. , #19690 ) ;
#17867 = CARTESIAN_POINT ( 'NONE',  ( 1.512611822017149166, 38.37995103523728346, 9.385845453595075938 ) ) ;
#17868 = ORIENTED_EDGE ( 'NONE', *, *, #9764, .F. ) ;
#17869 = FILL_AREA_STYLE ('',( #1984 ) ) ;
#17870 = CARTESIAN_POINT ( 'NONE',  ( 31.00000000000000711, 68.00000000000000000, -30.99999999999999289 ) ) ;
#17871 =( GEOMETRIC_REPRESENTATION_CONTEXT ( 3 ) GLOBAL_UNCERTAINTY_ASSIGNED_CONTEXT ( ( #4155 ) ) GLOBAL_UNIT_ASSIGNED_CONTEXT ( ( #15597, #7843, #17029 ) ) REPRESENTATION_CONTEXT ( 'NONE', 'WORKASPACE' ) );
#17872 = DIRECTION ( 'NONE',  ( -0.000000000000000000, 1.000000000000000000, -0.000000000000000000 ) ) ;
#17873 = ADVANCED_FACE ( 'NONE', ( #7674 ), #17352, .T. ) ;
#17874 = DIRECTION ( 'NONE',  ( 0.000000000000000000, 1.000000000000000000, -0.000000000000000000 ) ) ;
#17875 = VERTEX_POINT ( 'NONE', #6336 ) ;
#17876 = CARTESIAN_POINT ( 'NONE',  ( 458.8334540492693350, 242.8734308960556234, 0.000000000000000000 ) ) ;
#17877 =( NAMED_UNIT ( * ) PLANE_ANGLE_UNIT ( ) SI_UNIT ( $, .RADIAN. ) );
#17878 =( LENGTH_UNIT ( ) NAMED_UNIT ( * ) SI_UNIT ( .MILLI., .METRE. ) );
#17879 = ORIENTED_EDGE ( 'NONE', *, *, #13753, .T. ) ;
#17880 = CONICAL_SURFACE ( 'NONE', #8990, 13.89560290347679938, 1.567266246505109928 ) ;
#17881 = FILL_AREA_STYLE ('',( #14487 ) ) ;
#17882 = COLOUR_RGB ( '', 0.31764706, 0.68627451, 0.89019608) ;
#17883 = ORIENTED_EDGE ( 'NONE', *, *, #16170, .F. ) ;
#17884 = ORIENTED_EDGE ( 'NONE', *, *, #5476, .T. ) ;
#17885 = VECTOR ( 'NONE', #4007, 1000.000000000000000 ) ;
#17886 = ORIENTED_EDGE ( 'NONE', *, *, #115, .F. ) ;
#17887 =( NAMED_UNIT ( * ) SI_UNIT ( $, .STERADIAN. ) SOLID_ANGLE_UNIT ( ) );
#17888 =( REPRESENTATION_RELATIONSHIP ('NONE','NONE', #13279, #18121 ) REPRESENTATION_RELATIONSHIP_WITH_TRANSFORMATION ( #6647 )SHAPE_REPRESENTATION_RELATIONSHIP( ) );
#17889 = CARTESIAN_POINT ( 'NONE',  ( -1.000000000000015765, 147.7545334744432921, 491.0690926367356042 ) ) ;
#17890 = ORIENTED_EDGE ( 'NONE', *, *, #3948, .F. ) ;
#17891 = PLANE ( 'NONE',  #12676 ) ;
#17892 = DIRECTION ( 'NONE',  ( -1.000000000000000000, -0.000000000000000000, -0.000000000000000000 ) ) ;
#17893 = CIRCLE ( 'NONE', #6395, 1.000000000000000888 ) ;
#17894 = EDGE_LOOP ( 'NONE', ( #17836, #61, #971, #12691 ) ) ;
#17895 = CIRCLE ( 'NONE', #13620, 10.00000000000000888 ) ;
#17896 = CARTESIAN_POINT ( 'NONE',  ( 40.00000000000003553, -20.00000000000000000, 20.00000000000000355 ) ) ;
#17897 = CARTESIAN_POINT ( 'NONE',  ( -1.301042606982605321E-14, 140.1563709946295262, 488.5655098179835818 ) ) ;
#17898 = CARTESIAN_POINT ( 'NONE',  ( 463.8334540492693350, 191.8198460455371333, 225.0057801310552463 ) ) ;
#17899 = DIRECTION ( 'NONE',  ( 1.000000000000000000, -0.000000000000000000, 0.000000000000000000 ) ) ;
#17900 = PRESENTATION_LAYER_ASSIGNMENT (  '', '', ( #4399 ) ) ;
#17901 = PRESENTATION_LAYER_ASSIGNMENT (  '', '', ( #6059 ) ) ;
#17902 =( NAMED_UNIT ( * ) SI_UNIT ( $, .STERADIAN. ) SOLID_ANGLE_UNIT ( ) );
#17903 = PRESENTATION_LAYER_ASSIGNMENT (  '', '', ( #5412 ) ) ;
#17904 = DIRECTION ( 'NONE',  ( -1.000000000000000000, -0.000000000000000000, -0.000000000000000000 ) ) ;
#17905 = VECTOR ( 'NONE', #926, 1000.000000000000000 ) ;
#17906 = FACE_OUTER_BOUND ( 'NONE', #8550, .T. ) ;
#17907 = ORIENTED_EDGE ( 'NONE', *, *, #8862, .T. ) ;
#17908 = CARTESIAN_POINT ( 'NONE',  ( 2.181929469893224560, 140.4048636633015406, 499.8237260975781169 ) ) ;
#17909 = ORIENTED_EDGE ( 'NONE', *, *, #5741, .F. ) ;
#17910 = VECTOR ( 'NONE', #15241, 1000.000000000000000 ) ;
#17911 = EDGE_LOOP ( 'NONE', ( #8493, #17054, #3267, #9961 ) ) ;
#17912 = AXIS2_PLACEMENT_3D ( 'NONE', #7355, #1026, #13833 ) ;
#17913 = ORIENTED_EDGE ( 'NONE', *, *, #6892, .F. ) ;
#17914 = ORIENTED_EDGE ( 'NONE', *, *, #1664, .F. ) ;
#17915 = ORIENTED_EDGE ( 'NONE', *, *, #10375, .F. ) ;
#17916 = EDGE_CURVE ( 'NONE', #4707, #7627, #15216, .T. ) ;
#17917 = AXIS2_PLACEMENT_3D ( 'NONE', #8925, #2326, #18303 ) ;
#17918 = DIRECTION ( 'NONE',  ( 0.000000000000000000, 1.000000000000000000, 0.000000000000000000 ) ) ;
#17919 = CARTESIAN_POINT ( 'NONE',  ( 35.99999999999999289, 10.00000000000000000, 21.99999999999999645 ) ) ;
#17920 = DIRECTION ( 'NONE',  ( -0.000000000000000000, -1.000000000000000000, -0.000000000000000000 ) ) ;
#17921 = AXIS2_PLACEMENT_3D ( 'NONE', #9698, #6419, #3526 ) ;
#17922 = DIRECTION ( 'NONE',  ( 1.000000000000000000, 0.000000000000000000, -0.000000000000000000 ) ) ;
#17923 = CARTESIAN_POINT ( 'NONE',  ( 78.48937290013660117, 113.1299228374914208, 220.6387154965113382 ) ) ;
#17924 = FACE_OUTER_BOUND ( 'NONE', #1642, .T. ) ;
#17925 = VECTOR ( 'NONE', #19774, 1000.000000000000000 ) ;
#17926 = CARTESIAN_POINT ( 'NONE',  ( 153.4893729001366580, 145.9162550801369491, -140.0000000000001137 ) ) ;
#17927 = PLANE ( 'NONE',  #4862 ) ;
#17928 = MECHANICAL_DESIGN_GEOMETRIC_PRESENTATION_REPRESENTATION (  '', ( #6427 ), #13029 ) ;
#17929 = CARTESIAN_POINT ( 'NONE',  ( 111.4893729001366012, 125.7247684487574588, 254.0000000000000000 ) ) ;
#17930 = EDGE_CURVE ( 'NONE', #886, #12998, #4020, .T. ) ;
#17931 = DIRECTION ( 'NONE',  ( 1.000000000000000000, 2.135044278125300850E-16, -0.000000000000000000 ) ) ;
#17932 = VECTOR ( 'NONE', #1141, 1000.000000000000000 ) ;
#17933 = CARTESIAN_POINT ( 'NONE',  ( -33.99999999999997158, -20.00000000000000000, -22.99999999999999645 ) ) ;
#17934 = AXIS2_PLACEMENT_3D ( 'NONE', #15506, #3128, #1548 ) ;
#17935 = AXIS2_PLACEMENT_3D ( 'NONE', #7175, #10146, #562 ) ;
#17936 = EDGE_CURVE ( 'NONE', #20130, #4974, #4887, .T. ) ;
#17937 = EDGE_LOOP ( 'NONE', ( #17739, #3728 ) ) ;
#17938 = EDGE_CURVE ( 'NONE', #2920, #1752, #12516, .T. ) ;
#17939 = ORIENTED_EDGE ( 'NONE', *, *, #16983, .T. ) ;
#17940 = CIRCLE ( 'NONE', #11351, 3.883636366625808911 ) ;
#17941 = UNCERTAINTY_MEASURE_WITH_UNIT (LENGTH_MEASURE( 1.000000000000000082E-05 ), #19896, 'distance_accuracy_value', 'NONE');
#17942 = VERTEX_POINT ( 'NONE', #16141 ) ;
#17943 = ORIENTED_EDGE ( 'NONE', *, *, #2434, .T. ) ;
#17944 = EDGE_CURVE ( 'NONE', #17453, #15750, #19143, .T. ) ;
#17945 = UNCERTAINTY_MEASURE_WITH_UNIT (LENGTH_MEASURE( 1.000000000000000082E-05 ), #7797, 'distance_accuracy_value', 'NONE');
#17946 = DIRECTION ( 'NONE',  ( -1.000000000000000000, 0.000000000000000000, 0.000000000000000000 ) ) ;
#17947 = ORIENTED_EDGE ( 'NONE', *, *, #11865, .T. ) ;
#17948 = DIRECTION ( 'NONE',  ( 0.000000000000000000, 1.000000000000000000, 0.000000000000000000 ) ) ;
#17949 = LINE ( 'NONE', #19474, #16935 ) ;
#17950 = STYLED_ITEM ( 'NONE', ( #1961 ), #14788 ) ;
#17951 = CARTESIAN_POINT ( 'NONE',  ( 25.99999999999996092, 0.000000000000000000, -31.00000000000003197 ) ) ;
#17952 = FILL_AREA_STYLE ('',( #11466 ) ) ;
#17953 = FILL_AREA_STYLE ('',( #19297 ) ) ;
#17954 = MECHANICAL_DESIGN_GEOMETRIC_PRESENTATION_REPRESENTATION (  '', ( #4801 ), #16341 ) ;
#17955 = DIRECTION ( 'NONE',  ( -1.824549968389412905E-16, 1.000000000000000000, 0.000000000000000000 ) ) ;
#17956 = CARTESIAN_POINT ( 'NONE',  ( 4.899999999999999467, 12.00000000000000000, 0.000000000000000000 ) ) ;
#17957 = EDGE_CURVE ( 'NONE', #7830, #19379, #17757, .T. ) ;
#17958 = ORIENTED_EDGE ( 'NONE', *, *, #8890, .T. ) ;
#17959 = CARTESIAN_POINT ( 'NONE',  ( 34.00000000000002842, 3.000000000000000000, 26.00000000000000355 ) ) ;
#17960 = CYLINDRICAL_SURFACE ( 'NONE', #13324, 3.300000000000025135 ) ;
#17961 = CARTESIAN_POINT ( 'NONE',  ( 10.00000000000000000, 341.0487089519837696, -115.0000000000032969 ) ) ;
#17962 = AXIS2_PLACEMENT_3D ( 'NONE', #11479, #17863, #18340 ) ;
#17963 = DIRECTION ( 'NONE',  ( 0.000000000000000000, 1.000000000000000000, 0.000000000000000000 ) ) ;
#17964 = EDGE_CURVE ( 'NONE', #17228, #5650, #19088, .T. ) ;
#17965 = VERTEX_POINT ( 'NONE', #8192 ) ;
#17966 = EDGE_LOOP ( 'NONE', ( #12342, #1841, #7576, #240 ) ) ;
#17967 = EDGE_CURVE ( 'NONE', #11244, #3628, #1874, .T. ) ;
#17968 = DIRECTION ( 'NONE',  ( 1.000000000000000000, 0.000000000000000000, 0.000000000000000000 ) ) ;
#17969 = ORIENTED_EDGE ( 'NONE', *, *, #7588, .F. ) ;
#17970 = CARTESIAN_POINT ( 'NONE',  ( 31.00000000000003553, 11.00000000000000000, -26.00000000000000355 ) ) ;
#17971 = FACE_OUTER_BOUND ( 'NONE', #3153, .T. ) ;
#17972 = CIRCLE ( 'NONE', #19296, 10.00000000000000888 ) ;
#17973 = VERTEX_POINT ( 'NONE', #242 ) ;
#17974 = SURFACE_SIDE_STYLE ('',( #8496 ) ) ;
#17975 = CARTESIAN_POINT ( 'NONE',  ( 22.99999999999998224, 0.000000000000000000, -36.99999999999999289 ) ) ;
#17976 =( NAMED_UNIT ( * ) SI_UNIT ( $, .STERADIAN. ) SOLID_ANGLE_UNIT ( ) );
#17977 = COLOUR_RGB ( '', 0.40784314, 0.44705882, 0.49803922) ;
#17978 = CARTESIAN_POINT ( 'NONE',  ( -38.50085094405407204, 175.4489062796178871, 505.3921618609452935 ) ) ;
#17979 = CARTESIAN_POINT ( 'NONE',  ( 458.8334540492693350, 191.8198460455371333, 71.76606011801538898 ) ) ;
#17980 = EDGE_LOOP ( 'NONE', ( #18987, #13832, #2913, #10705 ) ) ;
#17981 = FACE_OUTER_BOUND ( 'NONE', #3116, .T. ) ;
#17982 =( NAMED_UNIT ( * ) SI_UNIT ( $, .STERADIAN. ) SOLID_ANGLE_UNIT ( ) );
#17983 = LINE ( 'NONE', #3876, #3749 ) ;
#17984 =( NAMED_UNIT ( * ) SI_UNIT ( $, .STERADIAN. ) SOLID_ANGLE_UNIT ( ) );
#17985 = SURFACE_SIDE_STYLE ('',( #2206 ) ) ;
#17986 = EDGE_CURVE ( 'NONE', #9564, #19183, #8089, .T. ) ;
#17987 = ORIENTED_EDGE ( 'NONE', *, *, #19325, .T. ) ;
#17988 = VECTOR ( 'NONE', #18385, 1000.000000000000000 ) ;
#17989 = VERTEX_POINT ( 'NONE', #11261 ) ;
#17990 = ORIENTED_EDGE ( 'NONE', *, *, #2812, .T. ) ;
#17991 = VERTEX_POINT ( 'NONE', #6544 ) ;
#17992 = DIRECTION ( 'NONE',  ( 0.000000000000000000, 0.000000000000000000, -1.000000000000000000 ) ) ;
#17993 = LINE ( 'NONE', #13385, #7804 ) ;
#17994 = VERTEX_POINT ( 'NONE', #9731 ) ;
#17995 = CARTESIAN_POINT ( 'NONE',  ( -23.00000000000002132, 6.000000000000000000, 37.00000000000000711 ) ) ;
#17996 = SURFACE_STYLE_USAGE ( .BOTH. , #9966 ) ;
#17997 =( NAMED_UNIT ( * ) PLANE_ANGLE_UNIT ( ) SI_UNIT ( $, .RADIAN. ) );
#17998 = CARTESIAN_POINT ( 'NONE',  ( 37.00000000000003553, 0.000000000000000000, 20.00000000000000000 ) ) ;
#17999 = DIRECTION ( 'NONE',  ( 0.000000000000000000, 0.5150380749100629263, 0.8571673007021070045 ) ) ;
#18000 = CARTESIAN_POINT ( 'NONE',  ( 53.48937290013660117, 77.72476844875745883, 250.0000000000000000 ) ) ;
#18001 = DIRECTION ( 'NONE',  ( 1.000000000000000000, 9.815121534730718631E-17, 0.000000000000000000 ) ) ;
#18002 = CARTESIAN_POINT ( 'NONE',  ( 3.850000000000000089, 14.27500000000000036, 0.000000000000000000 ) ) ;
#18003 = VERTEX_POINT ( 'NONE', #9933 ) ;
#18004 = UNCERTAINTY_MEASURE_WITH_UNIT (LENGTH_MEASURE( 1.000000000000000082E-05 ), #8674, 'distance_accuracy_value', 'NONE');
#18005 = PRESENTATION_STYLE_ASSIGNMENT (( #13104 ) ) ;
#18006 = DIRECTION ( 'NONE',  ( 0.000000000000000000, -0.000000000000000000, -1.000000000000000000 ) ) ;
#18007 = VERTEX_POINT ( 'NONE', #6650 ) ;
#18008 = VECTOR ( 'NONE', #5267, 1000.000000000000000 ) ;
#18009 = ORIENTED_EDGE ( 'NONE', *, *, #19508, .F. ) ;
#18010 = ORIENTED_EDGE ( 'NONE', *, *, #14654, .T. ) ;
#18011 = EDGE_CURVE ( 'NONE', #5553, #9832, #18813, .T. ) ;
#18012 = ORIENTED_EDGE ( 'NONE', *, *, #10412, .F. ) ;
#18013 = ORIENTED_EDGE ( 'NONE', *, *, #14318, .F. ) ;
#18014 =( NAMED_UNIT ( * ) PLANE_ANGLE_UNIT ( ) SI_UNIT ( $, .RADIAN. ) );
#18015 = FACE_OUTER_BOUND ( 'NONE', #18477, .T. ) ;
#18016 = DIRECTION ( 'NONE',  ( -0.000000000000000000, -1.000000000000000000, -0.000000000000000000 ) ) ;
#18017 = CIRCLE ( 'NONE', #249, 5.000000000000000888 ) ;
#18018 = PLANE ( 'NONE',  #3272 ) ;
#18019 = PRESENTATION_STYLE_ASSIGNMENT (( #16407 ) ) ;
#18020 = LINE ( 'NONE', #10880, #12687 ) ;
#18021 = CIRCLE ( 'NONE', #13746, 2.500000000000002220 ) ;
#18022 = LINE ( 'NONE', #13210, #18008 ) ;
#18023 = CARTESIAN_POINT ( 'NONE',  ( 36.99999999999999289, 0.000000000000000000, -22.99999999999999645 ) ) ;
#18024 = CARTESIAN_POINT ( 'NONE',  ( 53.48937290013658696, 119.5973956464515879, 280.0825295754780768 ) ) ;
#18025 = DIRECTION ( 'NONE',  ( 0.000000000000000000, -1.000000000000000000, 0.000000000000000000 ) ) ;
#18026 = ADVANCED_FACE ( 'NONE', ( #12938, #3448 ), #14368, .T. ) ;
#18027 = DIRECTION ( 'NONE',  ( 0.000000000000000000, 0.000000000000000000, -1.000000000000000000 ) ) ;
#18028 = ORIENTED_EDGE ( 'NONE', *, *, #13171, .T. ) ;
#18029 = EDGE_LOOP ( 'NONE', ( #15766, #7708, #14851, #9552 ) ) ;
#18030 = LINE ( 'NONE', #15259, #2135 ) ;
#18031 = ORIENTED_EDGE ( 'NONE', *, *, #14047, .F. ) ;
#18032 = ORIENTED_EDGE ( 'NONE', *, *, #5106, .T. ) ;
#18033 = ADVANCED_FACE ( 'NONE', ( #17664 ), #17546, .F. ) ;
#18034 = SURFACE_SIDE_STYLE ('',( #5284 ) ) ;
#18035 = CARTESIAN_POINT ( 'NONE',  ( -31.00000000000006395, 3.000000000000000000, -25.99999999999999645 ) ) ;
#18036 = EDGE_LOOP ( 'NONE', ( #977, #2393 ) ) ;
#18037 = FACE_OUTER_BOUND ( 'NONE', #1220, .T. ) ;
#18038 = FILL_AREA_STYLE ('',( #10123 ) ) ;
#18039 = FACE_OUTER_BOUND ( 'NONE', #2006, .T. ) ;
#18040 = EDGE_CURVE ( 'NONE', #14347, #9830, #8953, .T. ) ;
#18041 = CARTESIAN_POINT ( 'NONE',  ( 463.8334540492693350, 214.2156642432025251, 0.000000000000000000 ) ) ;
#18042 =( NAMED_UNIT ( * ) PLANE_ANGLE_UNIT ( ) SI_UNIT ( $, .RADIAN. ) );
#18043 = DIRECTION ( 'NONE',  ( -1.000000000000000000, 0.000000000000000000, 0.000000000000000000 ) ) ;
#18044 = AXIS2_PLACEMENT_3D ( 'NONE', #16041, #4573, #14144 ) ;
#18045 = ORIENTED_EDGE ( 'NONE', *, *, #10622, .T. ) ;
#18046 = CARTESIAN_POINT ( 'NONE',  ( -30.99999999999999289, 68.00000000000000000, 31.00000000000000000 ) ) ;
#18047 = FILL_AREA_STYLE ('',( #19391 ) ) ;
#18048 =( LENGTH_UNIT ( ) NAMED_UNIT ( * ) SI_UNIT ( .MILLI., .METRE. ) );
#18049 = EDGE_CURVE ( 'NONE', #6215, #11216, #6673, .T. ) ;
#18050 = ADVANCED_FACE ( 'NONE', ( #11930 ), #5850, .T. ) ;
#18051 = EDGE_LOOP ( 'NONE', ( #14291, #3656, #19171, #10159 ) ) ;
#18052 = ORIENTED_EDGE ( 'NONE', *, *, #9146, .F. ) ;
#18053 = VECTOR ( 'NONE', #11130, 1000.000000000000000 ) ;
#18054 = ADVANCED_FACE ( 'NONE', ( #1169 ), #8927, .F. ) ;
#18055 =( GEOMETRIC_REPRESENTATION_CONTEXT ( 3 ) GLOBAL_UNCERTAINTY_ASSIGNED_CONTEXT ( ( #19698 ) ) GLOBAL_UNIT_ASSIGNED_CONTEXT ( ( #4693, #14171, #355 ) ) REPRESENTATION_CONTEXT ( 'NONE', 'WORKASPACE' ) );
#18056 = CARTESIAN_POINT ( 'NONE',  ( 39.99999999999999289, 8.000000000000000000, 18.99999999999999645 ) ) ;
#18057 = CARTESIAN_POINT ( 'NONE',  ( 78.48937290013660117, 103.1299228374914065, 170.4174721992565082 ) ) ;
#18058 = VERTEX_POINT ( 'NONE', #7105 ) ;
#18059 = CARTESIAN_POINT ( 'NONE',  ( 0.000000000000000000, 0.000000000000000000, -150.0000000000000000 ) ) ;
#18060 = DIRECTION ( 'NONE',  ( 1.000000000000000000, 5.889072920838430686E-16, -0.000000000000000000 ) ) ;
#18061 = UNCERTAINTY_MEASURE_WITH_UNIT (LENGTH_MEASURE( 1.000000000000000082E-05 ), #2012, 'distance_accuracy_value', 'NONE');
#18062 = DIRECTION ( 'NONE',  ( 0.000000000000000000, 0.000000000000000000, -1.000000000000000000 ) ) ;
#18063 = ADVANCED_FACE ( 'NONE', ( #19727 ), #2743, .T. ) ;
#18064 = CARTESIAN_POINT ( 'NONE',  ( 0.000000000000000000, 147.7545334744432921, 496.6642397995874489 ) ) ;
#18065 = LINE ( 'NONE', #3966, #16638 ) ;
#18066 = ORIENTED_EDGE ( 'NONE', *, *, #15477, .F. ) ;
#18067 = LINE ( 'NONE', #11712, #1899 ) ;
#18068 = SURFACE_SIDE_STYLE ('',( #16851 ) ) ;
#18069 = DIRECTION ( 'NONE',  ( 1.000000000000000000, -0.000000000000000000, -0.000000000000000000 ) ) ;
#18070 = EDGE_CURVE ( 'NONE', #10437, #8331, #7197, .T. ) ;
#18071 = AXIS2_PLACEMENT_3D ( 'NONE', #3298, #2151, #5063 ) ;
#18072 =( GEOMETRIC_REPRESENTATION_CONTEXT ( 3 ) GLOBAL_UNCERTAINTY_ASSIGNED_CONTEXT ( ( #13289 ) ) GLOBAL_UNIT_ASSIGNED_CONTEXT ( ( #10789, #5602, #15187 ) ) REPRESENTATION_CONTEXT ( 'NONE', 'WORKASPACE' ) );
#18073 = VERTEX_POINT ( 'NONE', #15222 ) ;
#18074 = SURFACE_STYLE_USAGE ( .BOTH. , #12109 ) ;
#18075 = AXIS2_PLACEMENT_3D ( 'NONE', #15427, #18302, #1255 ) ;
#18076 = EDGE_CURVE ( 'NONE', #6572, #7832, #879, .T. ) ;
#18077 = VERTEX_POINT ( 'NONE', #5941 ) ;
#18078 = ORIENTED_EDGE ( 'NONE', *, *, #16951, .T. ) ;
#18079 = VERTEX_POINT ( 'NONE', #18094 ) ;
#18080 = VERTEX_POINT ( 'NONE', #15335 ) ;
#18081 = DIRECTION ( 'NONE',  ( -9.815121534730717399E-17, 1.000000000000000000, 0.000000000000000000 ) ) ;
#18082 = DIRECTION ( 'NONE',  ( 0.000000000000000000, -0.7071067811865475727, -0.7071067811865475727 ) ) ;
#18083 = EDGE_LOOP ( 'NONE', ( #9770, #7768 ) ) ;
#18084 =( GEOMETRIC_REPRESENTATION_CONTEXT ( 3 ) GLOBAL_UNCERTAINTY_ASSIGNED_CONTEXT ( ( #16588 ) ) GLOBAL_UNIT_ASSIGNED_CONTEXT ( ( #3892, #17997, #13389 ) ) REPRESENTATION_CONTEXT ( 'NONE', 'WORKASPACE' ) );
#18085 = SURFACE_STYLE_USAGE ( .BOTH. , #19250 ) ;
#18086 = CIRCLE ( 'NONE', #6938, 1.000000000000004219 ) ;
#18087 = FILL_AREA_STYLE_COLOUR ( '', #9613 ) ;
#18088 = DIRECTION ( 'NONE',  ( -1.000000000000000000, 0.000000000000000000, -0.000000000000000000 ) ) ;
#18089 = CARTESIAN_POINT ( 'NONE',  ( 111.4893729001366012, 122.8810204491430369, 322.0399576098686225 ) ) ;
#18090 = CARTESIAN_POINT ( 'NONE',  ( -0.7456292300257998384, 138.9173202923915653, 489.3604919264676596 ) ) ;
#18091 = SURFACE_STYLE_USAGE ( .BOTH. , #16579 ) ;
#18092 = CARTESIAN_POINT ( 'NONE',  ( 486.8117674897343363, 214.2156642432025251, 245.0000000000000000 ) ) ;
#18093 = EDGE_CURVE ( 'NONE', #5165, #3197, #18498, .T. ) ;
#18094 = CARTESIAN_POINT ( 'NONE',  ( 109.4893729001365870, 211.0574367717017594, 346.4752554294135507 ) ) ;
#18095 = LINE ( 'NONE', #1177, #2 ) ;
#18096 = ORIENTED_EDGE ( 'NONE', *, *, #19539, .F. ) ;
#18097 = EDGE_CURVE ( 'NONE', #9020, #3581, #4393, .T. ) ;
#18098 = AXIS2_PLACEMENT_3D ( 'NONE', #19854, #16604, #19749 ) ;
#18099 = VECTOR ( 'NONE', #11678, 1000.000000000000000 ) ;
#18100 =( GEOMETRIC_REPRESENTATION_CONTEXT ( 3 ) GLOBAL_UNCERTAINTY_ASSIGNED_CONTEXT ( ( #686 ) ) GLOBAL_UNIT_ASSIGNED_CONTEXT ( ( #915, #5489, #12083 ) ) REPRESENTATION_CONTEXT ( 'NONE', 'WORKASPACE' ) );
#18101 = ORIENTED_EDGE ( 'NONE', *, *, #1914, .T. ) ;
#18102 = PRODUCT_DEFINITION_CONTEXT ( 'detailed design', #8957, 'design' ) ;
#18103 = PRODUCT_DEFINITION_CONTEXT ( 'detailed design', #5268, 'design' ) ;
#18104 = VERTEX_POINT ( 'NONE', #7398 ) ;
#18105 = VERTEX_POINT ( 'NONE', #13682 ) ;
#18106 = DIRECTION ( 'NONE',  ( 0.000000000000000000, 1.000000000000000000, 0.000000000000000000 ) ) ;
#18107 = FACE_OUTER_BOUND ( 'NONE', #3635, .T. ) ;
#18108 = FACE_BOUND ( 'NONE', #11795, .T. ) ;
#18109 = DIRECTION ( 'NONE',  ( 1.000000000000000000, 2.135044278125300850E-16, -0.000000000000000000 ) ) ;
#18110 = VECTOR ( 'NONE', #4884, 1000.000000000000000 ) ;
#18111 = DIRECTION ( 'NONE',  ( -0.000000000000000000, -0.000000000000000000, 1.000000000000000000 ) ) ;
#18112 = DIRECTION ( 'NONE',  ( 0.000000000000000000, 0.000000000000000000, 1.000000000000000000 ) ) ;
#18113 = FILL_AREA_STYLE ('',( #8652 ) ) ;
#18114 = CARTESIAN_POINT ( 'NONE',  ( 22.99999999999998224, 10.00000000000000000, 37.00000000000000711 ) ) ;
#18115 = PLANE ( 'NONE',  #15256 ) ;
#18116 = CARTESIAN_POINT ( 'NONE',  ( -25.99999999999999645, 68.00000000000000000, -31.00000000000003197 ) ) ;
#18117 = EDGE_CURVE ( 'NONE', #12429, #14767, #12043, .T. ) ;
#18118 = FACE_OUTER_BOUND ( 'NONE', #10355, .T. ) ;
#18119 = DIRECTION ( 'NONE',  ( 0.000000000000000000, 1.000000000000000000, 0.000000000000000000 ) ) ;
#18120 = LINE ( 'NONE', #8659, #6751 ) ;
#18121 = SHAPE_REPRESENTATION ( 'Servo-Axe', ( #2741 ), #4080 ) ;
#18122 = VERTEX_POINT ( 'NONE', #16690 ) ;
#18123 = AXIS2_PLACEMENT_3D ( 'NONE', #1288, #1684, #15957 ) ;
#18124 = AXIS2_PLACEMENT_3D ( 'NONE', #12564, #9783, #5161 ) ;
#18125 = VECTOR ( 'NONE', #5060, 1000.000000000000000 ) ;
#18126 = ORIENTED_EDGE ( 'NONE', *, *, #12709, .F. ) ;
#18127 = VERTEX_POINT ( 'NONE', #19938 ) ;
#18128 = VERTEX_POINT ( 'NONE', #2539 ) ;
#18129 = SURFACE_SIDE_STYLE ('',( #7233 ) ) ;
#18130 = DIRECTION ( 'NONE',  ( 0.000000000000000000, 1.000000000000000000, 0.000000000000000000 ) ) ;
#18131 = DIRECTION ( 'NONE',  ( 1.000000000000000000, 5.889072920838430686E-16, -0.000000000000000000 ) ) ;
#18132 = EDGE_CURVE ( 'NONE', #3908, #4572, #4297, .T. ) ;
#18133 = CARTESIAN_POINT ( 'NONE',  ( -81.18192946989245229, 147.7545334744432921, 491.0690926367356042 ) ) ;
#18134 =( NAMED_UNIT ( * ) PLANE_ANGLE_UNIT ( ) SI_UNIT ( $, .RADIAN. ) );
#18135 = CARTESIAN_POINT ( 'NONE',  ( 30.99999999999999645, 68.00000000000000000, 31.00000000000001066 ) ) ;
#18136 = FILL_AREA_STYLE_COLOUR ( '', #2044 ) ;
#18137 = PRESENTATION_LAYER_ASSIGNMENT (  '', '', ( #12220 ) ) ;
#18138 = DIRECTION ( 'NONE',  ( 1.197852309262419498E-15, -1.000000000000000000, 0.000000000000000000 ) ) ;
#18139 = PLANE ( 'NONE',  #413 ) ;
#18140 = CARTESIAN_POINT ( 'NONE',  ( 0.3499999999999999778, -18.17500000000000071, 2.225795557450314789E-15 ) ) ;
#18141 =( NAMED_UNIT ( * ) SI_UNIT ( $, .STERADIAN. ) SOLID_ANGLE_UNIT ( ) );
#18142 = AXIS2_PLACEMENT_3D ( 'NONE', #17590, #6982, #9767 ) ;
#18143 = VERTEX_POINT ( 'NONE', #12643 ) ;
#18144 = DIRECTION ( 'NONE',  ( 0.000000000000000000, 0.000000000000000000, 1.000000000000000000 ) ) ;
#18145 = LINE ( 'NONE', #2593, #7382 ) ;
#18146 = ADVANCED_FACE ( 'NONE', ( #3163 ), #9443, .T. ) ;
#18147 = ORIENTED_EDGE ( 'NONE', *, *, #17936, .F. ) ;
#18148 = AXIS2_PLACEMENT_3D ( 'NONE', #2842, #10683, #12219 ) ;
#18149 = MECHANICAL_DESIGN_GEOMETRIC_PRESENTATION_REPRESENTATION (  '', ( #9594 ), #3024 ) ;
#18150 = ORIENTED_EDGE ( 'NONE', *, *, #3726, .F. ) ;
#18151 = EDGE_CURVE ( 'NONE', #16062, #2620, #7649, .T. ) ;
#18152 = CARTESIAN_POINT ( 'NONE',  ( 30.99999999999999645, 3.000000000000000000, 26.00000000000000355 ) ) ;
#18153 = CARTESIAN_POINT ( 'NONE',  ( -30.99999999999999289, 68.00000000000000000, 31.00000000000000000 ) ) ;
#18154 = UNCERTAINTY_MEASURE_WITH_UNIT (LENGTH_MEASURE( 1.000000000000000082E-05 ), #17747, 'distance_accuracy_value', 'NONE');
#18155 = ORIENTED_EDGE ( 'NONE', *, *, #8431, .T. ) ;
#18156 = CARTESIAN_POINT ( 'NONE',  ( 133.4893729001365728, 167.9162550801369491, 250.0000000000000000 ) ) ;
#18157 = CARTESIAN_POINT ( 'NONE',  ( -79.38291287507639993, 139.9432517092814692, 501.1364486412747397 ) ) ;
#18158 = FACE_OUTER_BOUND ( 'NONE', #13756, .T. ) ;
#18159 = CIRCLE ( 'NONE', #12931, 10.00000000000000888 ) ;
#18160 = ADVANCED_FACE ( 'NONE', ( #12754 ), #15752, .F. ) ;
#18161 = DIRECTION ( 'NONE',  ( 0.000000000000000000, 0.000000000000000000, -1.000000000000000000 ) ) ;
#18162 = PRESENTATION_STYLE_ASSIGNMENT (( #3665 ) ) ;
#18163 = CARTESIAN_POINT ( 'NONE',  ( 35.99999999999999289, 6.000000000000000000, 17.99999999999998934 ) ) ;
#18164 = CIRCLE ( 'NONE', #20133, 10.00000000000000888 ) ;
#18165 =( NAMED_UNIT ( * ) PLANE_ANGLE_UNIT ( ) SI_UNIT ( $, .RADIAN. ) );
#18166 =( GEOMETRIC_REPRESENTATION_CONTEXT ( 3 ) GLOBAL_UNCERTAINTY_ASSIGNED_CONTEXT ( ( #7042 ) ) GLOBAL_UNIT_ASSIGNED_CONTEXT ( ( #15339, #5944, #13398 ) ) REPRESENTATION_CONTEXT ( 'NONE', 'WORKASPACE' ) );
#18167 = VECTOR ( 'NONE', #19321, 1000.000000000000000 ) ;
#18168 = CARTESIAN_POINT ( 'NONE',  ( -31.81980515339462912, 11.00000000000000000, -31.81980515339465043 ) ) ;
#18169 = APPLICATION_PROTOCOL_DEFINITION ( 'draft international standard', 'automotive_design', 1998, #17633 ) ;
#18170 = EDGE_CURVE ( 'NONE', #14445, #2001, #4815, .T. ) ;
#18171 = ADVANCED_FACE ( 'NONE', ( #10990 ), #54, .F. ) ;
#18172 = ORIENTED_EDGE ( 'NONE', *, *, #1852, .F. ) ;
#18173 = AXIS2_PLACEMENT_3D ( 'NONE', #19498, #2096, #6554 ) ;
#18174 = ORIENTED_EDGE ( 'NONE', *, *, #6847, .T. ) ;
#18175 = ORIENTED_EDGE ( 'NONE', *, *, #7283, .F. ) ;
#18176 = AXIS2_PLACEMENT_3D ( 'NONE', #14168, #12435, #15646 ) ;
#18177 = ADVANCED_FACE ( 'NONE', ( #15431 ), #14278, .T. ) ;
#18178 = VECTOR ( 'NONE', #15168, 1000.000000000000000 ) ;
#18179 = ORIENTED_EDGE ( 'NONE', *, *, #7607, .T. ) ;
#18180 = EDGE_CURVE ( 'NONE', #15201, #20154, #10886, .T. ) ;
#18181 = FACE_OUTER_BOUND ( 'NONE', #1921, .T. ) ;
#18182 = ORIENTED_EDGE ( 'NONE', *, *, #1549, .T. ) ;
#18183 = DIRECTION ( 'NONE',  ( 1.000000000000000000, 0.000000000000000000, 0.000000000000000000 ) ) ;
#18184 = CIRCLE ( 'NONE', #8967, 10.00000000000000888 ) ;
#18185 = DIRECTION ( 'NONE',  ( 0.000000000000000000, 1.000000000000000000, 0.000000000000000000 ) ) ;
#18186 = VECTOR ( 'NONE', #9282, 1000.000000000000000 ) ;
#18187 = ORIENTED_EDGE ( 'NONE', *, *, #662, .F. ) ;
#18188 = EDGE_CURVE ( 'NONE', #17540, #6961, #3374, .T. ) ;
#18189 = DIRECTION ( 'NONE',  ( -0.000000000000000000, -0.000000000000000000, 1.000000000000000000 ) ) ;
#18190 = ADVANCED_FACE ( 'NONE', ( #1484 ), #14080, .F. ) ;
#18191 = CYLINDRICAL_SURFACE ( 'NONE', #11530, 2.999999999999999112 ) ;
#18192 = CARTESIAN_POINT ( 'NONE',  ( -1.301042606982605321E-14, 139.2066006846527841, 488.2525619656396429 ) ) ;
#18193 = DIRECTION ( 'NONE',  ( 1.000000000000000000, 0.000000000000000000, 0.000000000000000000 ) ) ;
#18194 = AXIS2_PLACEMENT_3D ( 'NONE', #6827, #13116, #19359 ) ;
#18195 = AXIS2_PLACEMENT_3D ( 'NONE', #18825, #17393, #14310 ) ;
#18196 = LINE ( 'NONE', #6903, #17047 ) ;
#18197 = FILL_AREA_STYLE_COLOUR ( '', #66 ) ;
#18198 = FACE_OUTER_BOUND ( 'NONE', #18315, .T. ) ;
#18199 = CARTESIAN_POINT ( 'NONE',  ( -75.00000000000000000, 313.8311070602663904, -142.2176018917206761 ) ) ;
#18200 = SURFACE_STYLE_FILL_AREA ( #5542 ) ;
#18201 = EDGE_CURVE ( 'NONE', #4515, #4998, #20349, .T. ) ;
#18202 = SURFACE_STYLE_FILL_AREA ( #10480 ) ;
#18203 = LINE ( 'NONE', #8932, #13176 ) ;
#18204 = CIRCLE ( 'NONE', #3069, 12.65000000000000036 ) ;
#18205 = ORIENTED_EDGE ( 'NONE', *, *, #12904, .F. ) ;
#18206 =( GEOMETRIC_REPRESENTATION_CONTEXT ( 3 ) GLOBAL_UNCERTAINTY_ASSIGNED_CONTEXT ( ( #1001 ) ) GLOBAL_UNIT_ASSIGNED_CONTEXT ( ( #13552, #2615, #947 ) ) REPRESENTATION_CONTEXT ( 'NONE', 'WORKASPACE' ) );
#18207 = PRESENTATION_LAYER_ASSIGNMENT (  '', '', ( #13948 ) ) ;
#18208 = CARTESIAN_POINT ( 'NONE',  ( 463.8334540492693350, 134.2156642432025251, 250.0000000000000000 ) ) ;
#18209 = ORIENTED_EDGE ( 'NONE', *, *, #17930, .T. ) ;
#18210 = EDGE_LOOP ( 'NONE', ( #3580, #10615, #16178, #16365, #5166, #13354, #12474, #5114, #7229, #7762, #14361, #8721 ) ) ;
#18211 = VECTOR ( 'NONE', #5006, 1000.000000000000000 ) ;
#18212 = VERTEX_POINT ( 'NONE', #20142 ) ;
#18213 =( GEOMETRIC_REPRESENTATION_CONTEXT ( 3 ) GLOBAL_UNCERTAINTY_ASSIGNED_CONTEXT ( ( #976 ) ) GLOBAL_UNIT_ASSIGNED_CONTEXT ( ( #19729, #15433, #13986 ) ) REPRESENTATION_CONTEXT ( 'NONE', 'WORKASPACE' ) );
#18214 = EDGE_CURVE ( 'NONE', #4998, #2140, #13270, .T. ) ;
#18215 =( NAMED_UNIT ( * ) SI_UNIT ( $, .STERADIAN. ) SOLID_ANGLE_UNIT ( ) );
#18216 = DIRECTION ( 'NONE',  ( 1.000000000000000000, -0.000000000000000000, 0.000000000000000000 ) ) ;
#18217 = PLANE ( 'NONE',  #7267 ) ;
#18218 = COLOUR_RGB ( '', 0.08235294, 0.09019608, 0.10196078) ;
#18219 = CYLINDRICAL_SURFACE ( 'NONE', #7876, 1.000000000000000888 ) ;
#18220 = EDGE_CURVE ( 'NONE', #13534, #9868, #6163, .T. ) ;
#18221 = CARTESIAN_POINT ( 'NONE',  ( -30.99999999999999645, 68.00000000000000000, -30.99999999999999289 ) ) ;
#18222 = CIRCLE ( 'NONE', #13006, 8.000000000000007105 ) ;
#18223 = LINE ( 'NONE', #4135, #12761 ) ;
#18224 = DIRECTION ( 'NONE',  ( 0.000000000000000000, 0.000000000000000000, 1.000000000000000000 ) ) ;
#18225 = DIRECTION ( 'NONE',  ( 1.000000000000000000, -0.000000000000000000, -0.000000000000000000 ) ) ;
#18226 = DIRECTION ( 'NONE',  ( -0.000000000000000000, -1.000000000000000000, -0.000000000000000000 ) ) ;
#18227 = CIRCLE ( 'NONE', #9347, 8.000000000000000000 ) ;
#18228 = CIRCLE ( 'NONE', #4759, 3.300000000000025135 ) ;
#18229 =( NAMED_UNIT ( * ) SI_UNIT ( $, .STERADIAN. ) SOLID_ANGLE_UNIT ( ) );
#18230 = AXIS2_PLACEMENT_3D ( 'NONE', #741, #1979, #7062 ) ;
#18231 = ORIENTED_EDGE ( 'NONE', *, *, #5608, .T. ) ;
#18232 = VECTOR ( 'NONE', #17680, 1000.000000000000000 ) ;
#18233 = CIRCLE ( 'NONE', #9361, 10.00000000000000888 ) ;
#18234 =( GEOMETRIC_REPRESENTATION_CONTEXT ( 3 ) GLOBAL_UNCERTAINTY_ASSIGNED_CONTEXT ( ( #19376 ) ) GLOBAL_UNIT_ASSIGNED_CONTEXT ( ( #19048, #2990, #6509 ) ) REPRESENTATION_CONTEXT ( 'NONE', 'WORKASPACE' ) );
#18235 = VERTEX_POINT ( 'NONE', #19413 ) ;
#18236 = VECTOR ( 'NONE', #3209, 1000.000000000000000 ) ;
#18237 = CARTESIAN_POINT ( 'NONE',  ( 463.8334540492693350, 214.2156642432025251, 250.0000000000000000 ) ) ;
#18238 = ORIENTED_EDGE ( 'NONE', *, *, #18703, .F. ) ;
#18239 = EDGE_LOOP ( 'NONE', ( #4165, #17096, #17100, #1991 ) ) ;
#18240 = VECTOR ( 'NONE', #16522, 1000.000000000000000 ) ;
#18241 = SURFACE_STYLE_FILL_AREA ( #8964 ) ;
#18242 = EDGE_CURVE ( 'NONE', #11435, #15883, #6970, .T. ) ;
#18243 = CARTESIAN_POINT ( 'NONE',  ( -35.00000000000000000, 19.00000000000000000, -21.00000000000000000 ) ) ;
#18244 = AXIS2_PLACEMENT_3D ( 'NONE', #10906, #12454, #4618 ) ;
#18245 = CARTESIAN_POINT ( 'NONE',  ( -31.81980515339462912, 0.000000000000000000, 31.81980515339465043 ) ) ;
#18246 = STYLED_ITEM ( 'NONE', ( #7766 ), #10481 ) ;
#18247 = DIRECTION ( 'NONE',  ( -0.000000000000000000, -1.000000000000000000, -0.000000000000000000 ) ) ;
#18248 =( NAMED_UNIT ( * ) SI_UNIT ( $, .STERADIAN. ) SOLID_ANGLE_UNIT ( ) );
#18249 = CARTESIAN_POINT ( 'NONE',  ( -1.387778780781445676E-14, 216.7545334744432921, 500.8237260975782874 ) ) ;
#18250 = FACE_OUTER_BOUND ( 'NONE', #4987, .T. ) ;
#18251 = VECTOR ( 'NONE', #1333, 1000.000000000000000 ) ;
#18252 = AXIS2_PLACEMENT_3D ( 'NONE', #6324, #17042, #12410 ) ;
#18253 = DIRECTION ( 'NONE',  ( 1.000000000000000000, 0.000000000000000000, 0.000000000000000000 ) ) ;
#18254 = CARTESIAN_POINT ( 'NONE',  ( -26.00000000000002842, 3.000000000000000000, -39.99999999999999289 ) ) ;
#18255 = LINE ( 'NONE', #8794, #338 ) ;
#18256 = PRESENTATION_LAYER_ASSIGNMENT (  '', '', ( #2477 ) ) ;
#18257 = DIRECTION ( 'NONE',  ( 0.000000000000000000, 0.000000000000000000, -1.000000000000000000 ) ) ;
#18258 = ORIENTED_EDGE ( 'NONE', *, *, #9245, .F. ) ;
#18259 = CARTESIAN_POINT ( 'NONE',  ( 30.99999999999999645, 0.000000000000000000, 26.00000000000000355 ) ) ;
#18260 =( NAMED_UNIT ( * ) SI_UNIT ( $, .STERADIAN. ) SOLID_ANGLE_UNIT ( ) );
#18261 = LINE ( 'NONE', #2385, #18558 ) ;
#18262 = AXIS2_PLACEMENT_3D ( 'NONE', #17640, #9812, #16121 ) ;
#18263 = VECTOR ( 'NONE', #11485, 1000.000000000000000 ) ;
#18264 = AXIS2_PLACEMENT_3D ( 'NONE', #15869, #6382, #5152 ) ;
#18265 = ORIENTED_EDGE ( 'NONE', *, *, #5253, .T. ) ;
#18266 = AXIS2_PLACEMENT_3D ( 'NONE', #2177, #16526, #16131 ) ;
#18267 = ADVANCED_FACE ( 'NONE', ( #8422 ), #12963, .T. ) ;
#18268 = VERTEX_POINT ( 'NONE', #12855 ) ;
#18269 = DIRECTION ( 'NONE',  ( -0.000000000000000000, -1.000000000000000000, -0.000000000000000000 ) ) ;
#18270 = DIRECTION ( 'NONE',  ( 1.000000000000000000, 0.000000000000000000, 0.000000000000000000 ) ) ;
#18271 = ORIENTED_EDGE ( 'NONE', *, *, #1240, .T. ) ;
#18272 = LINE ( 'NONE', #4061, #2618 ) ;
#18273 = CARTESIAN_POINT ( 'NONE',  ( -79.85426141749488238, 139.6565686763037206, 500.5947571826810076 ) ) ;
#18274 = STYLED_ITEM ( 'NONE', ( #17128 ), #2209 ) ;
#18275 = LINE ( 'NONE', #8707, #14913 ) ;
#18276 = AXIS2_PLACEMENT_3D ( 'NONE', #7978, #13969, #20248 ) ;
#18277 = DIRECTION ( 'NONE',  ( 0.000000000000000000, 0.000000000000000000, 1.000000000000000000 ) ) ;
#18278 = DIRECTION ( 'NONE',  ( 0.000000000000000000, 0.000000000000000000, 1.000000000000000000 ) ) ;
#18279 = CARTESIAN_POINT ( 'NONE',  ( 463.8334540492693350, 134.2156642432025251, -87.31255586191144857 ) ) ;
#18280 = VERTEX_POINT ( 'NONE', #570 ) ;
#18281 = DIRECTION ( 'NONE',  ( -0.000000000000000000, 1.000000000000000000, -0.000000000000000000 ) ) ;
#18282 = APPLICATION_CONTEXT ( 'automotive_design' ) ;
#18283 = DIRECTION ( 'NONE',  ( -0.000000000000000000, -1.000000000000000000, 0.000000000000000000 ) ) ;
#18284 = CARTESIAN_POINT ( 'NONE',  ( 2.999999999999996891, 60.00000000000000711, 6.000000000000000000 ) ) ;
#18285 = PRODUCT_CONTEXT ( 'NONE', #9860, 'mechanical' ) ;
#18286 = EDGE_LOOP ( 'NONE', ( #7911, #11477, #18878, #13910 ) ) ;
#18287 = CARTESIAN_POINT ( 'NONE',  ( -211.5106270998635409, 113.1299228374912502, 220.6387154965113382 ) ) ;
#18288 = EDGE_CURVE ( 'NONE', #5835, #19977, #14699, .T. ) ;
#18289 = ORIENTED_EDGE ( 'NONE', *, *, #7351, .F. ) ;
#18290 = ORIENTED_EDGE ( 'NONE', *, *, #14822, .F. ) ;
#18291 = AXIS2_PLACEMENT_3D ( 'NONE', #18846, #4756, #8251 ) ;
#18292 = ORIENTED_EDGE ( 'NONE', *, *, #17938, .F. ) ;
#18293 = AXIS2_PLACEMENT_3D ( 'NONE', #9271, #13912, #4750 ) ;
#18294 = CARTESIAN_POINT ( 'NONE',  ( -35.00000000000000000, 19.00000000000000000, 20.99999999999999289 ) ) ;
#18295 = ORIENTED_EDGE ( 'NONE', *, *, #5067, .F. ) ;
#18296 = CARTESIAN_POINT ( 'NONE',  ( -30.99999999999999645, 0.000000000000000000, -30.99999999999999289 ) ) ;
#18297 = ORIENTED_EDGE ( 'NONE', *, *, #10232, .F. ) ;
#18298 = FILL_AREA_STYLE ('',( #5841 ) ) ;
#18299 = EDGE_CURVE ( 'NONE', #14156, #3610, #13161, .T. ) ;
#18300 = SURFACE_STYLE_FILL_AREA ( #10376 ) ;
#18301 = PRESENTATION_STYLE_ASSIGNMENT (( #5935 ) ) ;
#18302 = DIRECTION ( 'NONE',  ( 0.000000000000000000, -1.000000000000000000, 0.000000000000000000 ) ) ;
#18303 = DIRECTION ( 'NONE',  ( 0.000000000000000000, 0.6235460666509320404, -0.7817866094812263578 ) ) ;
#18304 = EDGE_CURVE ( 'NONE', #8469, #4676, #6564, .T. ) ;
#18305 = CARTESIAN_POINT ( 'NONE',  ( 30.99999999999997158, 0.000000000000000000, 19.99999999999999289 ) ) ;
#18306 = DIRECTION ( 'NONE',  ( 0.000000000000000000, -1.000000000000000000, 0.000000000000000000 ) ) ;
#18307 =( NAMED_UNIT ( * ) PLANE_ANGLE_UNIT ( ) SI_UNIT ( $, .RADIAN. ) );
#18308 = VECTOR ( 'NONE', #5144, 1000.000000000000000 ) ;
#18309 = CARTESIAN_POINT ( 'NONE',  ( -82.18192946989275072, 138.7545334744432637, 499.8237260975782306 ) ) ;
#18310 = DIRECTION ( 'NONE',  ( 0.000000000000000000, 0.000000000000000000, -1.000000000000000000 ) ) ;
#18311 =( NAMED_UNIT ( * ) SI_UNIT ( $, .STERADIAN. ) SOLID_ANGLE_UNIT ( ) );
#18312 = ORIENTED_EDGE ( 'NONE', *, *, #11262, .F. ) ;
#18313 = EDGE_CURVE ( 'NONE', #12074, #12831, #16167, .T. ) ;
#18314 = EDGE_CURVE ( 'NONE', #12727, #14445, #16065, .T. ) ;
#18315 = EDGE_LOOP ( 'NONE', ( #9298, #7622, #16298, #17314 ) ) ;
#18316 = UNCERTAINTY_MEASURE_WITH_UNIT (LENGTH_MEASURE( 1.000000000000000082E-05 ), #18525, 'distance_accuracy_value', 'NONE');
#18317 = ORIENTED_EDGE ( 'NONE', *, *, #14713, .F. ) ;
#18318 = ORIENTED_EDGE ( 'NONE', *, *, #5419, .F. ) ;
#18319 = FACE_BOUND ( 'NONE', #12421, .T. ) ;
#18320 = CARTESIAN_POINT ( 'NONE',  ( 32.99999999999998579, 8.000000000000000000, 25.99999999999999645 ) ) ;
#18321 = DIRECTION ( 'NONE',  ( 0.000000000000000000, 1.000000000000000000, -0.000000000000000000 ) ) ;
#18322 = ADVANCED_FACE ( 'NONE', ( #14386 ), #6111, .F. ) ;
#18323 = FILL_AREA_STYLE_COLOUR ( '', #6060 ) ;
#18324 = FILL_AREA_STYLE_COLOUR ( '', #4259 ) ;
#18325 = CYLINDRICAL_SURFACE ( 'NONE', #17327, 2.500000000000002220 ) ;
#18326 = PLANE ( 'NONE',  #3141 ) ;
#18327 = SURFACE_STYLE_FILL_AREA ( #10598 ) ;
#18328 = LINE ( 'NONE', #13417, #5606 ) ;
#18329 = ADVANCED_FACE ( 'NONE', ( #4763 ), #12702, .T. ) ;
#18330 = CARTESIAN_POINT ( 'NONE',  ( 0.000000000000000000, -3.000000000000000000, 0.000000000000000000 ) ) ;
#18331 = STYLED_ITEM ( 'NONE', ( #14222 ), #3760 ) ;
#18332 = LINE ( 'NONE', #10414, #5310 ) ;
#18333 = CARTESIAN_POINT ( 'NONE',  ( 35.00000000000003553, 3.000000000000000000, -18.49999999999999645 ) ) ;
#18334 = EDGE_CURVE ( 'NONE', #664, #9734, #1312, .T. ) ;
#18335 = ORIENTED_EDGE ( 'NONE', *, *, #5814, .T. ) ;
#18336 = CARTESIAN_POINT ( 'NONE',  ( 10.00000000000000000, 306.0487089519837127, -150.0000000000038369 ) ) ;
#18337 = ORIENTED_EDGE ( 'NONE', *, *, #12710, .T. ) ;
#18338 = VERTEX_POINT ( 'NONE', #14123 ) ;
#18339 = VECTOR ( 'NONE', #18976, 1000.000000000000000 ) ;
#18340 = DIRECTION ( 'NONE',  ( 0.000000000000000000, 0.000000000000000000, -1.000000000000000000 ) ) ;
#18341 = DIRECTION ( 'NONE',  ( 1.000000000000000000, 0.000000000000000000, 0.000000000000000000 ) ) ;
#18342 = UNCERTAINTY_MEASURE_WITH_UNIT (LENGTH_MEASURE( 1.000000000000000082E-05 ), #18048, 'distance_accuracy_value', 'NONE');
#18343 = AXIS2_PLACEMENT_3D ( 'NONE', #17606, #9778, #16088 ) ;
#18344 = LINE ( 'NONE', #12266, #15857 ) ;
#18345 = DIRECTION ( 'NONE',  ( -8.673617379884027583E-16, 0.000000000000000000, -1.000000000000000000 ) ) ;
#18346 = DIRECTION ( 'NONE',  ( 0.000000000000000000, 1.000000000000000000, 0.000000000000000000 ) ) ;
#18347 = EDGE_CURVE ( 'NONE', #10821, #14143, #15012, .T. ) ;
#18348 = CARTESIAN_POINT ( 'NONE',  ( 35.00000000000003553, 0.000000000000000000, -20.99999999999999645 ) ) ;
#18349 = CARTESIAN_POINT ( 'NONE',  ( -79.99999999999995737, 216.7545334744432921, 510.3921618609452935 ) ) ;
#18350 = CARTESIAN_POINT ( 'NONE',  ( 0.000000000000000000, 10.00000000000000000, 0.000000000000000000 ) ) ;
#18351 = CARTESIAN_POINT ( 'NONE',  ( -33.99999999999997158, -20.00000000000000000, -25.99999999999999645 ) ) ;
#18352 = ORIENTED_EDGE ( 'NONE', *, *, #17250, .F. ) ;
#18353 = FILL_AREA_STYLE ('',( #5095 ) ) ;
#18354 = PRESENTATION_STYLE_ASSIGNMENT (( #8983 ) ) ;
#18355 = EDGE_CURVE ( 'NONE', #11036, #975, #18852, .T. ) ;
#18356 = LINE ( 'NONE', #19787, #783 ) ;
#18357 = VECTOR ( 'NONE', #15430, 1000.000000000000000 ) ;
#18358 = ORIENTED_EDGE ( 'NONE', *, *, #18943, .F. ) ;
#18359 = UNCERTAINTY_MEASURE_WITH_UNIT (LENGTH_MEASURE( 1.000000000000000082E-05 ), #1504, 'distance_accuracy_value', 'NONE');
#18360 = EDGE_LOOP ( 'NONE', ( #17120, #5225, #6981, #8438 ) ) ;
#18361 = FILL_AREA_STYLE_COLOUR ( '', #1273 ) ;
#18362 = ORIENTED_EDGE ( 'NONE', *, *, #15301, .T. ) ;
#18363 = FACE_OUTER_BOUND ( 'NONE', #3368, .T. ) ;
#18364 = PLANE ( 'NONE',  #19521 ) ;
#18365 = ADVANCED_FACE ( 'NONE', ( #1430 ), #20201, .F. ) ;
#18366 = FILL_AREA_STYLE_COLOUR ( '', #17583 ) ;
#18367 = CIRCLE ( 'NONE', #2895, 10.00000000000000888 ) ;
#18368 = CARTESIAN_POINT ( 'NONE',  ( -80.37285363047544706, 140.5927919537299715, 501.0285821077172841 ) ) ;
#18369 = SURFACE_STYLE_FILL_AREA ( #15303 ) ;
#18370 = CARTESIAN_POINT ( 'NONE',  ( -3.000000000000001776, 40.80057950988138771, 9.013878188659973034 ) ) ;
#18371 = ORIENTED_EDGE ( 'NONE', *, *, #9427, .T. ) ;
#18372 = DIRECTION ( 'NONE',  ( 0.000000000000000000, 1.000000000000000000, -0.000000000000000000 ) ) ;
#18373 = CARTESIAN_POINT ( 'NONE',  ( 53.48937290013658696, 113.1299228374914065, 170.4174721992565082 ) ) ;
#18374 = APPLICATION_PROTOCOL_DEFINITION ( 'draft international standard', 'automotive_design', 1998, #19702 ) ;
#18375 = EDGE_CURVE ( 'NONE', #12596, #1145, #11047, .T. ) ;
#18376 = ORIENTED_EDGE ( 'NONE', *, *, #40, .T. ) ;
#18377 = CARTESIAN_POINT ( 'NONE',  ( -23.00000000000002132, 6.000000000000000000, 37.00000000000000711 ) ) ;
#18378 = EDGE_LOOP ( 'NONE', ( #18150, #17471, #14933, #12162 ) ) ;
#18379 = ORIENTED_EDGE ( 'NONE', *, *, #14435, .F. ) ;
#18380 = CIRCLE ( 'NONE', #8199, 3.300000000000004263 ) ;
#18381 = MECHANICAL_DESIGN_GEOMETRIC_PRESENTATION_REPRESENTATION (  '', ( #18725 ), #18055 ) ;
#18382 = EDGE_LOOP ( 'NONE', ( #4601, #13958, #13131, #16995 ) ) ;
#18383 = DIRECTION ( 'NONE',  ( -0.000000000000000000, -0.000000000000000000, 1.000000000000000000 ) ) ;
#18384 = EDGE_LOOP ( 'NONE', ( #17695, #8319, #16005, #2070 ) ) ;
#18385 = DIRECTION ( 'NONE',  ( -0.000000000000000000, -0.000000000000000000, 1.000000000000000000 ) ) ;
#18386 = SURFACE_SIDE_STYLE ('',( #1059 ) ) ;
#18387 = DIRECTION ( 'NONE',  ( -0.000000000000000000, -0.000000000000000000, 1.000000000000000000 ) ) ;
#18388 = LINE ( 'NONE', #9224, #10525 ) ;
#18389 = AXIS2_PLACEMENT_3D ( 'NONE', #12252, #10504, #7525 ) ;
#18390 = SURFACE_STYLE_FILL_AREA ( #9131 ) ;
#18391 = EDGE_CURVE ( 'NONE', #10186, #9635, #1628, .T. ) ;
#18392 = COLOUR_RGB ( '', 0.40784314, 0.44705882, 0.49803922) ;
#18393 = FACE_BOUND ( 'NONE', #13563, .T. ) ;
#18394 = CIRCLE ( 'NONE', #931, 1.000000000000000888 ) ;
#18395 = LINE ( 'NONE', #877, #19872 ) ;
#18396 = AXIS2_PLACEMENT_3D ( 'NONE', #6558, #15647, #11396 ) ;
#18397 = DIRECTION ( 'NONE',  ( -1.000000000000000000, -0.000000000000000000, -0.000000000000000000 ) ) ;
#18398 = CARTESIAN_POINT ( 'NONE',  ( 20.99999999999996092, -20.00000000000000000, 37.50000000000001421 ) ) ;
#18399 =( NAMED_UNIT ( * ) PLANE_ANGLE_UNIT ( ) SI_UNIT ( $, .RADIAN. ) );
#18400 = FILL_AREA_STYLE_COLOUR ( '', #1783 ) ;
#18401 = PRESENTATION_STYLE_ASSIGNMENT (( #20039 ) ) ;
#18402 = FILL_AREA_STYLE_COLOUR ( '', #3288 ) ;
#18403 = LINE ( 'NONE', #19841, #1011 ) ;
#18404 = PRESENTATION_STYLE_ASSIGNMENT (( #4212 ) ) ;
#18405 = ORIENTED_EDGE ( 'NONE', *, *, #2391, .F. ) ;
#18406 = EDGE_CURVE ( 'NONE', #15108, #7485, #11278, .T. ) ;
#18407 = VECTOR ( 'NONE', #12227, 1000.000000000000000 ) ;
#18408 = ORIENTED_EDGE ( 'NONE', *, *, #15181, .F. ) ;
#18409 = VECTOR ( 'NONE', #11699, 1000.000000000000000 ) ;
#18410 = ADVANCED_FACE ( 'NONE', ( #17511 ), #9803, .F. ) ;
#18411 = VERTEX_POINT ( 'NONE', #14340 ) ;
#18412 = EDGE_LOOP ( 'NONE', ( #6062, #15968 ) ) ;
#18413 = DIRECTION ( 'NONE',  ( -0.000000000000000000, -1.000000000000000000, -0.000000000000000000 ) ) ;
#18414 =( NAMED_UNIT ( * ) PLANE_ANGLE_UNIT ( ) SI_UNIT ( $, .RADIAN. ) );
#18415 =( NAMED_UNIT ( * ) SI_UNIT ( $, .STERADIAN. ) SOLID_ANGLE_UNIT ( ) );
#18416 = ORIENTED_EDGE ( 'NONE', *, *, #7414, .F. ) ;
#18417 = CARTESIAN_POINT ( 'NONE',  ( -211.5106270998635409, 113.1299228374912502, 79.58252780074349175 ) ) ;
#18418 = DIRECTION ( 'NONE',  ( 1.000000000000000000, 5.889072920838430686E-16, -0.000000000000000000 ) ) ;
#18419 = SURFACE_SIDE_STYLE ('',( #2556 ) ) ;
#18420 = SURFACE_SIDE_STYLE ('',( #18327 ) ) ;
#18421 = ADVANCED_FACE ( 'NONE', ( #13485 ), #16213, .T. ) ;
#18422 = STYLED_ITEM ( 'NONE', ( #13462 ), #16744 ) ;
#18423 = CARTESIAN_POINT ( 'NONE',  ( 53.48937290013660828, 34.32473510485366575, -140.0000000000001137 ) ) ;
#18424 = AXIS2_PLACEMENT_3D ( 'NONE', #19552, #18321, #602 ) ;
#18425 =( LENGTH_UNIT ( ) NAMED_UNIT ( * ) SI_UNIT ( .MILLI., .METRE. ) );
#18426 = CIRCLE ( 'NONE', #8547, 3.000000000000002665 ) ;
#18427 = CARTESIAN_POINT ( 'NONE',  ( 3.500000000000000000, 0.000000000000000000, 0.000000000000000000 ) ) ;
#18428 = DIRECTION ( 'NONE',  ( -0.000000000000000000, -1.000000000000000000, 0.000000000000000000 ) ) ;
#18429 = EDGE_CURVE ( 'NONE', #8375, #5650, #5641, .T. ) ;
#18430 = ORIENTED_EDGE ( 'NONE', *, *, #3308, .F. ) ;
#18431 = VERTEX_POINT ( 'NONE', #9696 ) ;
#18432 = ORIENTED_EDGE ( 'NONE', *, *, #16349, .T. ) ;
#18433 = ORIENTED_EDGE ( 'NONE', *, *, #12804, .T. ) ;
#18434 = ADVANCED_FACE ( 'NONE', ( #11547 ), #14644, .T. ) ;
#18435 = EDGE_LOOP ( 'NONE', ( #3578, #8242, #17890, #14753 ) ) ;
#18436 = ORIENTED_EDGE ( 'NONE', *, *, #1797, .T. ) ;
#18437 = VECTOR ( 'NONE', #9603, 1000.000000000000000 ) ;
#18438 = EDGE_CURVE ( 'NONE', #10947, #11436, #6724, .T. ) ;
#18439 = AXIS2_PLACEMENT_3D ( 'NONE', #2167, #11772, #14750 ) ;
#18440 = VECTOR ( 'NONE', #17243, 1000.000000000000000 ) ;
#18441 = CARTESIAN_POINT ( 'NONE',  ( 34.99999999999997868, 11.00000000000000000, -40.00000000000000711 ) ) ;
#18442 = DIRECTION ( 'NONE',  ( 1.000000000000000000, 0.000000000000000000, 0.000000000000000000 ) ) ;
#18443 = CARTESIAN_POINT ( 'NONE',  ( 498.8117674897343932, 191.8198460455371333, 225.0057801310552463 ) ) ;
#18444 = EDGE_CURVE ( 'NONE', #3235, #7373, #6832, .T. ) ;
#18445 = CARTESIAN_POINT ( 'NONE',  ( 53.48937290013659407, 145.9162550801369491, 0.000000000000000000 ) ) ;
#18446 =( NAMED_UNIT ( * ) PLANE_ANGLE_UNIT ( ) SI_UNIT ( $, .RADIAN. ) );
#18447 = ADVANCED_FACE ( 'NONE', ( #3525 ), #19364, .T. ) ;
#18448 = DIRECTION ( 'NONE',  ( 0.000000000000000000, 0.000000000000000000, -1.000000000000000000 ) ) ;
#18449 = DIRECTION ( 'NONE',  ( -1.000000000000000000, 0.000000000000000000, -0.000000000000000000 ) ) ;
#18450 = DIRECTION ( 'NONE',  ( 0.000000000000000000, 1.000000000000000000, 0.000000000000000000 ) ) ;
#18451 = VERTEX_POINT ( 'NONE', #15025 ) ;
#18452 =( NAMED_UNIT ( * ) SI_UNIT ( $, .STERADIAN. ) SOLID_ANGLE_UNIT ( ) );
#18453 = LINE ( 'NONE', #20205, #11659 ) ;
#18454 = DIRECTION ( 'NONE',  ( 0.000000000000000000, 0.000000000000000000, -1.000000000000000000 ) ) ;
#18455 = AXIS2_PLACEMENT_3D ( 'NONE', #19027, #14104, #9616 ) ;
#18456 = AXIS2_PLACEMENT_3D ( 'NONE', #18543, #1113, #15159 ) ;
#18457 = ORIENTED_EDGE ( 'NONE', *, *, #5096, .F. ) ;
#18458 = VERTEX_POINT ( 'NONE', #19165 ) ;
#18459 = ADVANCED_FACE ( 'NONE', ( #18198 ), #4103, .F. ) ;
#18460 = DIRECTION ( 'NONE',  ( 1.000000000000000000, -0.000000000000000000, -0.000000000000000000 ) ) ;
#18461 = COLOUR_RGB ( '', 0.09019608, 0.27058824, 0.51372549) ;
#18462 = PRESENTATION_STYLE_ASSIGNMENT (( #12186 ) ) ;
#18463 = VERTEX_POINT ( 'NONE', #13985 ) ;
#18464 = CARTESIAN_POINT ( 'NONE',  ( -32.00000000000000711, 6.000000000000000000, -22.00000000000000355 ) ) ;
#18465 = CARTESIAN_POINT ( 'NONE',  ( -79.14393569841020337, 140.2407135942496268, 501.6205206800881342 ) ) ;
#18466 = EDGE_CURVE ( 'NONE', #4537, #18431, #12125, .T. ) ;
#18467 = EDGE_CURVE ( 'NONE', #7322, #11810, #11958, .T. ) ;
#18468 = CARTESIAN_POINT ( 'NONE',  ( 32.99999999999998579, 8.000000000000000000, 21.99999999999999645 ) ) ;
#18469 = CARTESIAN_POINT ( 'NONE',  ( -35.00000000000000000, 19.00000000000000000, 20.99999999999999289 ) ) ;
#18470 = FILL_AREA_STYLE ('',( #4787 ) ) ;
#18471 = EDGE_LOOP ( 'NONE', ( #1956, #10066, #4746, #17657 ) ) ;
#18472 = DIRECTION ( 'NONE',  ( 7.719519468096785259E-14, 0.000000000000000000, 1.000000000000000000 ) ) ;
#18473 = SURFACE_SIDE_STYLE ('',( #2910 ) ) ;
#18474 = CARTESIAN_POINT ( 'NONE',  ( 40.00000000000000000, 68.00000000000000000, 26.00000000000000355 ) ) ;
#18475 = PRODUCT_CONTEXT ( 'NONE', #12370, 'mechanical' ) ;
#18476 = ORIENTED_EDGE ( 'NONE', *, *, #18695, .F. ) ;
#18477 = EDGE_LOOP ( 'NONE', ( #7573, #4800, #12886, #14440 ) ) ;
#18478 = DIRECTION ( 'NONE',  ( 0.000000000000000000, 0.000000000000000000, 1.000000000000000000 ) ) ;
#18479 = ORIENTED_EDGE ( 'NONE', *, *, #1258, .F. ) ;
#18480 = AXIS2_PLACEMENT_3D ( 'NONE', #9514, #18782, #37 ) ;
#18481 = ORIENTED_EDGE ( 'NONE', *, *, #16724, .F. ) ;
#18482 =( GEOMETRIC_REPRESENTATION_CONTEXT ( 3 ) GLOBAL_UNCERTAINTY_ASSIGNED_CONTEXT ( ( #18359 ) ) GLOBAL_UNIT_ASSIGNED_CONTEXT ( ( #1504, #275, #9551 ) ) REPRESENTATION_CONTEXT ( 'NONE', 'WORKASPACE' ) );
#18483 = ORIENTED_EDGE ( 'NONE', *, *, #17411, .F. ) ;
#18484 = CARTESIAN_POINT ( 'NONE',  ( -81.00000000000127898, 216.7545334744432921, 489.5655098179835818 ) ) ;
#18485 = ORIENTED_EDGE ( 'NONE', *, *, #6871, .T. ) ;
#18486 = CARTESIAN_POINT ( 'NONE',  ( -79.99999999999995737, 216.7545334744432921, 205.1946179577815883 ) ) ;
#18487 = ORIENTED_EDGE ( 'NONE', *, *, #1655, .F. ) ;
#18488 = PRESENTATION_STYLE_ASSIGNMENT (( #10374 ) ) ;
#18489 = ADVANCED_FACE ( 'NONE', ( #15123 ), #1170, .F. ) ;
#18490 = CARTESIAN_POINT ( 'NONE',  ( 43.00000000000001421, 0.000000000000000000, -150.0000000000000000 ) ) ;
#18491 = DIRECTION ( 'NONE',  ( 1.000000000000000000, 5.889072920838430686E-16, -0.000000000000000000 ) ) ;
#18492 = VECTOR ( 'NONE', #18940, 1000.000000000000000 ) ;
#18493 = CARTESIAN_POINT ( 'NONE',  ( -26.00000000000002842, 3.000000000000000000, -31.00000000000003197 ) ) ;
#18494 = DIRECTION ( 'NONE',  ( 0.000000000000000000, 1.000000000000000000, 0.000000000000000000 ) ) ;
#18495 = CARTESIAN_POINT ( 'NONE',  ( -58.16843972078500258, 319.7545334744432353, 485.1700099148404206 ) ) ;
#18496 = VECTOR ( 'NONE', #18189, 1000.000000000000000 ) ;
#18497 = CARTESIAN_POINT ( 'NONE',  ( -211.5106270998635409, 123.1299228374912644, 220.6387154965113382 ) ) ;
#18498 = LINE ( 'NONE', #5749, #16244 ) ;
#18499 = LINE ( 'NONE', #12221, #8655 ) ;
#18500 = DIRECTION ( 'NONE',  ( 0.000000000000000000, 0.000000000000000000, 1.000000000000000000 ) ) ;
#18501 = CYLINDRICAL_SURFACE ( 'NONE', #253, 2.500000000000002220 ) ;
#18502 = TOROIDAL_SURFACE ( 'NONE', #15902, 8.000000000000000000, 1.000000000000000000 ) ;
#18503 =( NAMED_UNIT ( * ) PLANE_ANGLE_UNIT ( ) SI_UNIT ( $, .RADIAN. ) );
#18504 = AXIS2_PLACEMENT_3D ( 'NONE', #19891, #4451, #16642 ) ;
#18505 = CARTESIAN_POINT ( 'NONE',  ( 498.8117674897343932, 191.8198460455371333, 34.99421986894476788 ) ) ;
#18506 = ORIENTED_EDGE ( 'NONE', *, *, #10629, .T. ) ;
#18507 = ORIENTED_EDGE ( 'NONE', *, *, #18070, .T. ) ;
#18508 = STYLED_ITEM ( 'NONE', ( #17651 ), #13886 ) ;
#18509 = VERTEX_POINT ( 'NONE', #1261 ) ;
#18510 = COLOUR_RGB ( '', 0.66274510, 0.83137255, 0.94901961) ;
#18511 = ORIENTED_EDGE ( 'NONE', *, *, #5977, .T. ) ;
#18512 = DIRECTION ( 'NONE',  ( 0.000000000000000000, 0.000000000000000000, 1.000000000000000000 ) ) ;
#18513 = VERTEX_POINT ( 'NONE', #2639 ) ;
#18514 = DIRECTION ( 'NONE',  ( -0.000000000000000000, -1.000000000000000000, -0.000000000000000000 ) ) ;
#18515 = FACE_OUTER_BOUND ( 'NONE', #18051, .T. ) ;
#18516 = LINE ( 'NONE', #7309, #18541 ) ;
#18517 = COLOUR_RGB ( '', 0.31764706, 0.68627451, 0.89019608) ;
#18518 = ORIENTED_EDGE ( 'NONE', *, *, #18922, .T. ) ;
#18519 = SURFACE_SIDE_STYLE ('',( #3063 ) ) ;
#18520 = DIRECTION ( 'NONE',  ( -0.000000000000000000, -1.000000000000000000, -0.000000000000000000 ) ) ;
#18521 = CARTESIAN_POINT ( 'NONE',  ( 3.850000000000000089, 0.000000000000000000, 0.000000000000000000 ) ) ;
#18522 = SURFACE_SIDE_STYLE ('',( #7127 ) ) ;
#18523 = SURFACE_SIDE_STYLE ('',( #5781 ) ) ;
#18524 = VECTOR ( 'NONE', #17026, 1000.000000000000000 ) ;
#18525 =( LENGTH_UNIT ( ) NAMED_UNIT ( * ) SI_UNIT ( .MILLI., .METRE. ) );
#18526 =( LENGTH_UNIT ( ) NAMED_UNIT ( * ) SI_UNIT ( .MILLI., .METRE. ) );
#18527 = AXIS2_PLACEMENT_3D ( 'NONE', #6276, #70, #15863 ) ;
#18528 = CARTESIAN_POINT ( 'NONE',  ( 40.00000000000000000, 68.00000000000000000, -25.99999999999999645 ) ) ;
#18529 = DIRECTION ( 'NONE',  ( 1.000000000000000000, 0.000000000000000000, 0.000000000000000000 ) ) ;
#18530 = AXIS2_PLACEMENT_3D ( 'NONE', #13914, #5794, #4154 ) ;
#18531 = AXIS2_PLACEMENT_3D ( 'NONE', #6641, #11858, #18224 ) ;
#18532 = EDGE_CURVE ( 'NONE', #11769, #11321, #6164, .T. ) ;
#18533 = ORIENTED_EDGE ( 'NONE', *, *, #6922, .T. ) ;
#18534 = VERTEX_POINT ( 'NONE', #15223 ) ;
#18535 = CARTESIAN_POINT ( 'NONE',  ( -75.00000000000000000, 313.8311070602663904, -142.2176018917206761 ) ) ;
#18536 = ORIENTED_EDGE ( 'NONE', *, *, #16344, .F. ) ;
#18537 = ORIENTED_EDGE ( 'NONE', *, *, #15557, .T. ) ;
#18538 = VECTOR ( 'NONE', #6992, 1000.000000000000000 ) ;
#18539 = VECTOR ( 'NONE', #1687, 1000.000000000000000 ) ;
#18540 = CYLINDRICAL_SURFACE ( 'NONE', #6454, 9.000000000000007105 ) ;
#18541 = VECTOR ( 'NONE', #13594, 1000.000000000000000 ) ;
#18542 = UNCERTAINTY_MEASURE_WITH_UNIT (LENGTH_MEASURE( 1.000000000000000082E-05 ), #9073, 'distance_accuracy_value', 'NONE');
#18543 = CARTESIAN_POINT ( 'NONE',  ( 458.8334540492693350, 191.8198460455371333, 168.2339398819845826 ) ) ;
#18544 = PLANE ( 'NONE',  #2967 ) ;
#18545 = DIRECTION ( 'NONE',  ( 0.000000000000000000, 0.000000000000000000, -1.000000000000000000 ) ) ;
#18547 = EDGE_CURVE ( 'NONE', #16123, #10884, #14252, .T. ) ;
#18546 = SURFACE_STYLE_USAGE ( .BOTH. , #11132 ) ;
#18548 = AXIS2_PLACEMENT_3D ( 'NONE', #1844, #8154, #17209 ) ;
#18549 = LINE ( 'NONE', #1118, #15245 ) ;
#18550 = CIRCLE ( 'NONE', #9353, 10.00000000000000888 ) ;
#18551 = SURFACE_STYLE_FILL_AREA ( #19779 ) ;
#18552 = DIRECTION ( 'NONE',  ( 0.000000000000000000, 0.000000000000000000, 1.000000000000000000 ) ) ;
#18553 = DIRECTION ( 'NONE',  ( 0.000000000000000000, -1.000000000000000000, 0.000000000000000000 ) ) ;
#18554 = ADVANCED_FACE ( 'NONE', ( #10684 ), #5942, .F. ) ;
#18555 = ORIENTED_EDGE ( 'NONE', *, *, #3948, .T. ) ;
#18556 = PRESENTATION_STYLE_ASSIGNMENT (( #12279 ) ) ;
#18557 = DIRECTION ( 'NONE',  ( 1.000000000000000000, 0.000000000000000000, 0.000000000000000000 ) ) ;
#18558 = VECTOR ( 'NONE', #846, 1000.000000000000000 ) ;
#18559 = FACE_BOUND ( 'NONE', #997, .T. ) ;
#18560 = AXIS2_PLACEMENT_3D ( 'NONE', #17326, #20199, #15486 ) ;
#18561 = EDGE_CURVE ( 'NONE', #15692, #18007, #12440, .T. ) ;
#18562 = VECTOR ( 'NONE', #17032, 1000.000000000000000 ) ;
#18563 = AXIS2_PLACEMENT_3D ( 'NONE', #12688, #16912, #10722 ) ;
#18564 = VECTOR ( 'NONE', #18746, 1000.000000000000000 ) ;
#18565 = EDGE_LOOP ( 'NONE', ( #3240, #4199 ) ) ;
#18566 = EDGE_CURVE ( 'NONE', #15475, #2111, #2744, .T. ) ;
#18567 = CIRCLE ( 'NONE', #9693, 3.283624802691453848 ) ;
#18568 = LINE ( 'NONE', #16567, #60 ) ;
#18569 = ORIENTED_EDGE ( 'NONE', *, *, #6559, .T. ) ;
#18570 = CIRCLE ( 'NONE', #16320, 3.000000000000002665 ) ;
#18571 = DIRECTION ( 'NONE',  ( -1.000000000000000000, -0.000000000000000000, -0.000000000000000000 ) ) ;
#18572 = VECTOR ( 'NONE', #6212, 1000.000000000000000 ) ;
#18573 = CARTESIAN_POINT ( 'NONE',  ( 31.00000000000003553, 8.000000000000000000, 20.99999999999999289 ) ) ;
#18574 = ORIENTED_EDGE ( 'NONE', *, *, #6231, .F. ) ;
#18575 = CARTESIAN_POINT ( 'NONE',  ( 53.48937290013658696, 119.5973956464515879, 280.0825295754780768 ) ) ;
#18576 =( NAMED_UNIT ( * ) PLANE_ANGLE_UNIT ( ) SI_UNIT ( $, .RADIAN. ) );
#18577 = CIRCLE ( 'NONE', #12339, 18.49999999999998934 ) ;
#18579 = EDGE_CURVE ( 'NONE', #11398, #16195, #10300, .T. ) ;
#18578 =( LENGTH_UNIT ( ) NAMED_UNIT ( * ) SI_UNIT ( .MILLI., .METRE. ) );
#18580 = DIRECTION ( 'NONE',  ( 0.000000000000000000, 1.000000000000000000, 0.000000000000000000 ) ) ;
#18581 = FACE_OUTER_BOUND ( 'NONE', #2854, .T. ) ;
#18582 = AXIS2_PLACEMENT_3D ( 'NONE', #19464, #8064, #5379 ) ;
#18583 = LINE ( 'NONE', #18977, #2966 ) ;
#18584 = CYLINDRICAL_SURFACE ( 'NONE', #9699, 4.999999999999997335 ) ;
#18585 = VECTOR ( 'NONE', #14711, 1000.000000000000000 ) ;
#18586 = ORIENTED_EDGE ( 'NONE', *, *, #4611, .T. ) ;
#18587 = SURFACE_STYLE_USAGE ( .BOTH. , #7273 ) ;
#18588 = DIRECTION ( 'NONE',  ( 0.000000000000000000, 1.000000000000000000, 0.000000000000000000 ) ) ;
#18589 = CARTESIAN_POINT ( 'NONE',  ( -36.00000000000000711, 10.00000000000000000, -22.00000000000000355 ) ) ;
#18590 = PRODUCT_CONTEXT ( 'NONE', #19702, 'mechanical' ) ;
#18591 = VECTOR ( 'NONE', #11110, 1000.000000000000000 ) ;
#18592 = EDGE_CURVE ( 'NONE', #17811, #12058, #18499, .T. ) ;
#18593 = EDGE_LOOP ( 'NONE', ( #19765, #14518, #17479, #291 ) ) ;
#18594 = ORIENTED_EDGE ( 'NONE', *, *, #15797, .T. ) ;
#18595 = PRESENTATION_STYLE_ASSIGNMENT (( #9608 ) ) ;
#18596 = VECTOR ( 'NONE', #17851, 1000.000000000000000 ) ;
#18597 = ORIENTED_EDGE ( 'NONE', *, *, #3627, .F. ) ;
#18598 = VECTOR ( 'NONE', #3042, 1000.000000000000000 ) ;
#18599 = EDGE_CURVE ( 'NONE', #6961, #17540, #19175, .T. ) ;
#18600 = ORIENTED_EDGE ( 'NONE', *, *, #15707, .T. ) ;
#18601 = CIRCLE ( 'NONE', #4127, 12.00000000000000000 ) ;
#18602 = ORIENTED_EDGE ( 'NONE', *, *, #10266, .T. ) ;
#18603 = VECTOR ( 'NONE', #8179, 1000.000000000000000 ) ;
#18604 = CARTESIAN_POINT ( 'NONE',  ( 23.00000000000000711, 68.00000000000000000, -31.00000000000002487 ) ) ;
#18605 = ORIENTED_EDGE ( 'NONE', *, *, #14296, .F. ) ;
#18606 = PLANE ( 'NONE',  #464 ) ;
#18607 = VECTOR ( 'NONE', #13670, 1000.000000000000000 ) ;
#18608 = DIRECTION ( 'NONE',  ( 1.000000000000000000, 0.000000000000000000, 0.000000000000000000 ) ) ;
#18609 = LINE ( 'NONE', #2735, #4 ) ;
#18610 = CARTESIAN_POINT ( 'NONE',  ( 82.88953019741013861, 80.91625508013694912, 250.0000000000000000 ) ) ;
#18611 = CARTESIAN_POINT ( 'NONE',  ( 498.8117674897343932, 134.2156642432025251, 250.0000000000000000 ) ) ;
#18612 = DIRECTION ( 'NONE',  ( -1.000000000000000000, -0.000000000000000000, -0.000000000000000000 ) ) ;
#18613 = CARTESIAN_POINT ( 'NONE',  ( 1.163414457778310218E-15, 63.00000000000000000, 9.500000000000000000 ) ) ;
#18614 = EDGE_CURVE ( 'NONE', #17048, #16024, #2940, .T. ) ;
#18615 = DIRECTION ( 'NONE',  ( -0.000000000000000000, -0.000000000000000000, 1.000000000000000000 ) ) ;
#18616 = DIRECTION ( 'NONE',  ( 1.000000000000000000, 0.000000000000000000, -0.000000000000000000 ) ) ;
#18617 = DIRECTION ( 'NONE',  ( 1.000000000000000000, 0.000000000000000000, 0.000000000000000000 ) ) ;
#18618 = LINE ( 'NONE', #17277, #18598 ) ;
#18619 = DIRECTION ( 'NONE',  ( 1.000000000000000000, 0.000000000000000000, 0.000000000000000000 ) ) ;
#18620 = CONICAL_SURFACE ( 'NONE', #5151, 18.17500000000000071, 0.7483780475235185525 ) ;
#18621 = PRESENTATION_STYLE_ASSIGNMENT (( #15341 ) ) ;
#18622 = CARTESIAN_POINT ( 'NONE',  ( 0.4333752514400535105, 138.7761994944360424, 490.4323031634212953 ) ) ;
#18623 = FACE_OUTER_BOUND ( 'NONE', #12763, .T. ) ;
#18624 = ORIENTED_EDGE ( 'NONE', *, *, #19057, .F. ) ;
#18625 = VECTOR ( 'NONE', #6298, 1000.000000000000000 ) ;
#18626 = ORIENTED_EDGE ( 'NONE', *, *, #18956, .F. ) ;
#18627 = ORIENTED_EDGE ( 'NONE', *, *, #4038, .F. ) ;
#18628 = ORIENTED_EDGE ( 'NONE', *, *, #9762, .F. ) ;
#18629 = FILL_AREA_STYLE_COLOUR ( '', #20114 ) ;
#18630 = CARTESIAN_POINT ( 'NONE',  ( -80.85741104738939100, 138.7723821175181627, 490.5025619656437357 ) ) ;
#18631 = VERTEX_POINT ( 'NONE', #16985 ) ;
#18632 = AXIS2_PLACEMENT_3D ( 'NONE', #807, #16309, #5557 ) ;
#18633 = DIRECTION ( 'NONE',  ( -0.4740998230350218501, 0.8804710999221728729, 0.000000000000000000 ) ) ;
#18634 = SURFACE_STYLE_FILL_AREA ( #19750 ) ;
#18635 = ORIENTED_EDGE ( 'NONE', *, *, #19281, .F. ) ;
#18636 = CARTESIAN_POINT ( 'NONE',  ( 78.48937290013660117, 145.9162550801369491, 250.0000000000000000 ) ) ;
#18637 = CIRCLE ( 'NONE', #11735, 12.64814671169700055 ) ;
#18638 = CARTESIAN_POINT ( 'NONE',  ( -37.00000000000000711, 6.000000000000000000, 23.00000000000000000 ) ) ;
#18639 = DIRECTION ( 'NONE',  ( 1.000000000000000000, -0.000000000000000000, 0.000000000000000000 ) ) ;
#18640 = ORIENTED_EDGE ( 'NONE', *, *, #16735, .T. ) ;
#18641 = FACE_OUTER_BOUND ( 'NONE', #4404, .T. ) ;
#18642 = CARTESIAN_POINT ( 'NONE',  ( 0.000000000000000000, -3.000000000000000888, -150.0000000000000000 ) ) ;
#18643 = DIRECTION ( 'NONE',  ( -0.000000000000000000, -1.000000000000000000, -0.000000000000000000 ) ) ;
#18644 = SURFACE_STYLE_FILL_AREA ( #5972 ) ;
#18645 = EDGE_CURVE ( 'NONE', #6682, #17548, #966, .T. ) ;
#18646 = VERTEX_POINT ( 'NONE', #9135 ) ;
#18647 = AXIS2_PLACEMENT_3D ( 'NONE', #7681, #10468, #4382 ) ;
#18648 = ORIENTED_EDGE ( 'NONE', *, *, #12814, .F. ) ;
#18649 = ORIENTED_EDGE ( 'NONE', *, *, #4740, .F. ) ;
#18650 = PRESENTATION_STYLE_ASSIGNMENT (( #17204 ) ) ;
#18651 = ORIENTED_EDGE ( 'NONE', *, *, #12010, .T. ) ;
#18652 = EDGE_LOOP ( 'NONE', ( #6525, #16972, #17681, #4813, #6835 ) ) ;
#18653 = ORIENTED_EDGE ( 'NONE', *, *, #3211, .F. ) ;
#18654 = LINE ( 'NONE', #1112, #9654 ) ;
#18655 = DIRECTION ( 'NONE',  ( 0.000000000000000000, -0.000000000000000000, 1.000000000000000000 ) ) ;
#18656 =( NAMED_UNIT ( * ) SI_UNIT ( $, .STERADIAN. ) SOLID_ANGLE_UNIT ( ) );
#18657 = CARTESIAN_POINT ( 'NONE',  ( 143.0892156028631348, 80.91625508013694912, 250.0000000000000000 ) ) ;
#18658 = FACE_OUTER_BOUND ( 'NONE', #15688, .T. ) ;
#18659 = EDGE_CURVE ( 'NONE', #18463, #8369, #15432, .T. ) ;
#18660 = CARTESIAN_POINT ( 'NONE',  ( 53.48937290013660828, 127.7247684487574304, 357.7985149490353933 ) ) ;
#18661 = DIRECTION ( 'NONE',  ( 0.000000000000000000, 1.000000000000000000, 0.000000000000000000 ) ) ;
#18662 = ORIENTED_EDGE ( 'NONE', *, *, #13783, .T. ) ;
#18663 = LINE ( 'NONE', #14510, #15119 ) ;
#18664 = CARTESIAN_POINT ( 'NONE',  ( 458.8334540492693350, 0.000000000000000000, 250.0000000000000000 ) ) ;
#18665 = SURFACE_STYLE_FILL_AREA ( #6515 ) ;
#18666 = EDGE_CURVE ( 'NONE', #10931, #4636, #13872, .T. ) ;
#18667 = VECTOR ( 'NONE', #8946, 1000.000000000000000 ) ;
#18668 = ORIENTED_EDGE ( 'NONE', *, *, #16951, .F. ) ;
#18669 = APPLICATION_CONTEXT ( 'automotive_design' ) ;
#18670 = DIRECTION ( 'NONE',  ( -0.000000000000000000, -1.000000000000000000, -0.000000000000000000 ) ) ;
#18671 = EDGE_CURVE ( 'NONE', #16276, #18431, #5697, .T. ) ;
#18672 = ORIENTED_EDGE ( 'NONE', *, *, #4766, .F. ) ;
#18673 = CARTESIAN_POINT ( 'NONE',  ( 5.941205806953520074, 0.000000000000000000, 0.000000000000000000 ) ) ;
#18674 = ORIENTED_EDGE ( 'NONE', *, *, #6643, .T. ) ;
#18675 = CARTESIAN_POINT ( 'NONE',  ( 111.4893729001366154, 77.72476844875745883, 252.0000000000000000 ) ) ;
#18676 = FILL_AREA_STYLE_COLOUR ( '', #3796 ) ;
#18677 = VECTOR ( 'NONE', #12414, 1000.000000000000000 ) ;
#18678 = DIRECTION ( 'NONE',  ( 7.714700791774628163E-14, 0.000000000000000000, 1.000000000000000000 ) ) ;
#18679 = CARTESIAN_POINT ( 'NONE',  ( 406.3334540492693350, 167.8734308960555950, 250.0000000000000000 ) ) ;
#18680 = DIRECTION ( 'NONE',  ( 0.000000000000000000, 0.000000000000000000, 1.000000000000000000 ) ) ;
#18681 = VECTOR ( 'NONE', #7294, 1000.000000000000000 ) ;
#18682 = EDGE_LOOP ( 'NONE', ( #10694, #5422, #17987, #2025 ) ) ;
#18683 = CARTESIAN_POINT ( 'NONE',  ( -37.00000000000000000, 68.00000000000000000, 23.00000000000000355 ) ) ;
#18684 = ADVANCED_FACE ( 'NONE', ( #14485 ), #8345, .T. ) ;
#18685 = FILL_AREA_STYLE_COLOUR ( '', #9682 ) ;
#18686 = VERTEX_POINT ( 'NONE', #17374 ) ;
#18687 = VERTEX_POINT ( 'NONE', #6465 ) ;
#18688 = DIRECTION ( 'NONE',  ( 0.000000000000000000, 1.000000000000000000, 0.000000000000000000 ) ) ;
#18689 = ORIENTED_EDGE ( 'NONE', *, *, #7765, .T. ) ;
#18690 = ORIENTED_EDGE ( 'NONE', *, *, #9880, .T. ) ;
#18691 = EDGE_CURVE ( 'NONE', #19482, #11967, #4700, .T. ) ;
#18692 = ORIENTED_EDGE ( 'NONE', *, *, #19443, .F. ) ;
#18693 = CARTESIAN_POINT ( 'NONE',  ( -25.99999999999999645, 0.000000000000000000, 40.00000000000002132 ) ) ;
#18694 = AXIS2_PLACEMENT_3D ( 'NONE', #15005, #7180, #3668 ) ;
#18695 = EDGE_CURVE ( 'NONE', #3146, #12515, #8114, .T. ) ;
#18696 = ORIENTED_EDGE ( 'NONE', *, *, #14694, .T. ) ;
#18697 = CARTESIAN_POINT ( 'NONE',  ( 0.3830880647780208204, 140.5989314160965762, 501.0334628959610654 ) ) ;
#18698 = EDGE_CURVE ( 'NONE', #3441, #8286, #14279, .T. ) ;
#18699 = DIRECTION ( 'NONE',  ( 0.000000000000000000, 1.000000000000000000, 0.000000000000000000 ) ) ;
#18700 = FACE_OUTER_BOUND ( 'NONE', #17911, .T. ) ;
#18701 = FILL_AREA_STYLE ('',( #6157 ) ) ;
#18702 = CARTESIAN_POINT ( 'NONE',  ( -31.81980515339462912, 8.000000000000000000, 31.81980515339465043 ) ) ;
#18703 = EDGE_CURVE ( 'NONE', #16028, #12290, #4908, .T. ) ;
#18704 = CARTESIAN_POINT ( 'NONE',  ( -19.00000000000001776, 8.000000000000000000, 36.00000000000000711 ) ) ;
#18705 = DIRECTION ( 'NONE',  ( -0.000000000000000000, -1.000000000000000000, 0.000000000000000000 ) ) ;
#18706 = ORIENTED_EDGE ( 'NONE', *, *, #18170, .T. ) ;
#18707 = EDGE_CURVE ( 'NONE', #3672, #19445, #19196, .T. ) ;
#18708 = DIRECTION ( 'NONE',  ( 0.000000000000000000, 0.000000000000000000, 1.000000000000000000 ) ) ;
#18709 = FILL_AREA_STYLE ('',( #6051 ) ) ;
#18710 = DIRECTION ( 'NONE',  ( 0.000000000000000000, 1.000000000000000000, 0.000000000000000000 ) ) ;
#18711 = CARTESIAN_POINT ( 'NONE',  ( 486.8117674897343363, 214.2156642432025251, 245.0000000000000000 ) ) ;
#18712 = DIRECTION ( 'NONE',  ( 0.000000000000000000, -1.000000000000000000, 0.000000000000000000 ) ) ;
#18713 = DIRECTION ( 'NONE',  ( -0.000000000000000000, -1.000000000000000000, -0.000000000000000000 ) ) ;
#18714 = PLANE ( 'NONE',  #14130 ) ;
#18715 = ORIENTED_EDGE ( 'NONE', *, *, #14371, .F. ) ;
#18716 = VERTEX_POINT ( 'NONE', #9337 ) ;
#18717 = EDGE_LOOP ( 'NONE', ( #795, #19243 ) ) ;
#18718 = ORIENTED_EDGE ( 'NONE', *, *, #4532, .T. ) ;
#18719 = CARTESIAN_POINT ( 'NONE',  ( 40.00000000000000711, 11.00000000000000000, 34.99999999999997868 ) ) ;
#18720 = CARTESIAN_POINT ( 'NONE',  ( -80.44547052777866725, 138.7779086090105523, 490.4200269341494050 ) ) ;
#18721 = MECHANICAL_DESIGN_GEOMETRIC_PRESENTATION_REPRESENTATION (  '', ( #3965 ), #339 ) ;
#18722 = DIRECTION ( 'NONE',  ( -1.000000000000000000, -0.000000000000000000, -0.000000000000000000 ) ) ;
#18723 = STYLED_ITEM ( 'NONE', ( #18556 ), #5118 ) ;
#18724 = CARTESIAN_POINT ( 'NONE',  ( 498.8117674897343932, 191.8198460455371333, 91.76606011801541740 ) ) ;
#18725 = STYLED_ITEM ( 'NONE', ( #12849 ), #10935 ) ;
#18726 = VERTEX_POINT ( 'NONE', #15653 ) ;
#18727 = ADVANCED_FACE ( 'NONE', ( #3363 ), #11092, .F. ) ;
#18728 = CARTESIAN_POINT ( 'NONE',  ( -81.18192946989245229, 139.7545334744432637, 491.0690926367356042 ) ) ;
#18729 = DIRECTION ( 'NONE',  ( -1.000000000000000000, -0.000000000000000000, -8.673617379884027583E-16 ) ) ;
#18730 = ORIENTED_EDGE ( 'NONE', *, *, #19124, .T. ) ;
#18731 = EDGE_CURVE ( 'NONE', #7061, #16045, #55, .T. ) ;
#18732 = DIRECTION ( 'NONE',  ( 0.000000000000000000, 1.000000000000000000, 0.000000000000000000 ) ) ;
#18733 = CARTESIAN_POINT ( 'NONE',  ( 0.000000000000000000, 10.00000000000000000, 0.000000000000000000 ) ) ;
#18734 = ORIENTED_EDGE ( 'NONE', *, *, #8328, .T. ) ;
#18735 = DIRECTION ( 'NONE',  ( 1.445602896647338128E-15, 0.000000000000000000, 1.000000000000000000 ) ) ;
#18736 = CARTESIAN_POINT ( 'NONE',  ( 30.99999999999997513, 10.00000000000000000, 25.99999999999999645 ) ) ;
#18737 =( GEOMETRIC_REPRESENTATION_CONTEXT ( 3 ) GLOBAL_UNCERTAINTY_ASSIGNED_CONTEXT ( ( #13220 ) ) GLOBAL_UNIT_ASSIGNED_CONTEXT ( ( #5455, #14813, #14724 ) ) REPRESENTATION_CONTEXT ( 'NONE', 'WORKASPACE' ) );
#18738 = CIRCLE ( 'NONE', #2265, 5.000000000000000888 ) ;
#18739 = ORIENTED_EDGE ( 'NONE', *, *, #19260, .T. ) ;
#18740 = ORIENTED_EDGE ( 'NONE', *, *, #17711, .T. ) ;
#18741 = ORIENTED_EDGE ( 'NONE', *, *, #8396, .T. ) ;
#18742 = ORIENTED_EDGE ( 'NONE', *, *, #16803, .T. ) ;
#18743 = ORIENTED_EDGE ( 'NONE', *, *, #11177, .T. ) ;
#18744 = ORIENTED_EDGE ( 'NONE', *, *, #16352, .T. ) ;
#18745 =( LENGTH_UNIT ( ) NAMED_UNIT ( * ) SI_UNIT ( .MILLI., .METRE. ) );
#18746 = DIRECTION ( 'NONE',  ( -6.263247009234063646E-17, 0.6381222063396385646, -0.7699350945217602327 ) ) ;
#18747 = DIRECTION ( 'NONE',  ( 0.000000000000000000, 1.000000000000000000, 0.000000000000000000 ) ) ;
#18748 = MECHANICAL_DESIGN_GEOMETRIC_PRESENTATION_REPRESENTATION (  '', ( #15482 ), #19719 ) ;
#18749 = CYLINDRICAL_SURFACE ( 'NONE', #16354, 10.00000000000001066 ) ;
#18750 = VECTOR ( 'NONE', #9869, 1000.000000000000000 ) ;
#18751 = VERTEX_POINT ( 'NONE', #7896 ) ;
#18752 = EDGE_CURVE ( 'NONE', #4636, #2567, #9639, .T. ) ;
#18753 = CARTESIAN_POINT ( 'NONE',  ( 0.000000000000000000, 138.7545334744432637, 487.3411705753777596 ) ) ;
#18754 = CIRCLE ( 'NONE', #11862, 4.999999999999997335 ) ;
#18755 = CARTESIAN_POINT ( 'NONE',  ( -79.99999999999995737, 216.7545334744432921, 515.1946179577817020 ) ) ;
#18756 = LINE ( 'NONE', #18851, #15230 ) ;
#18757 = ORIENTED_EDGE ( 'NONE', *, *, #15833, .T. ) ;
#18758 = SURFACE_STYLE_USAGE ( .BOTH. , #18965 ) ;
#18759 = CARTESIAN_POINT ( 'NONE',  ( -40.00000000000000000, 68.00000000000000000, -25.99999999999999645 ) ) ;
#18760 = AXIS2_PLACEMENT_3D ( 'NONE', #7131, #19864, #16801 ) ;
#18761 =( GEOMETRIC_REPRESENTATION_CONTEXT ( 3 ) GLOBAL_UNCERTAINTY_ASSIGNED_CONTEXT ( ( #7466 ) ) GLOBAL_UNIT_ASSIGNED_CONTEXT ( ( #12633, #7988, #9436 ) ) REPRESENTATION_CONTEXT ( 'NONE', 'WORKASPACE' ) );
#18762 = VECTOR ( 'NONE', #19654, 1000.000000000000000 ) ;
#18763 = ORIENTED_EDGE ( 'NONE', *, *, #11280, .F. ) ;
#18764 = DIRECTION ( 'NONE',  ( 1.000000000000000000, 5.889072920838430686E-16, -0.000000000000000000 ) ) ;
#18765 = VECTOR ( 'NONE', #19363, 1000.000000000000000 ) ;
#18766 = ORIENTED_EDGE ( 'NONE', *, *, #3241, .F. ) ;
#18767 = SURFACE_STYLE_FILL_AREA ( #1543 ) ;
#18768 =( NAMED_UNIT ( * ) PLANE_ANGLE_UNIT ( ) SI_UNIT ( $, .RADIAN. ) );
#18769 = ORIENTED_EDGE ( 'NONE', *, *, #7097, .F. ) ;
#18770 = CARTESIAN_POINT ( 'NONE',  ( 5.950000000000000178, -12.65000000000000036, -1.701720561796546765E-15 ) ) ;
#18771 = DIRECTION ( 'NONE',  ( -0.000000000000000000, -1.000000000000000000, -0.000000000000000000 ) ) ;
#18772 = AXIS2_PLACEMENT_3D ( 'NONE', #7369, #11809, #15307 ) ;
#18773 = CARTESIAN_POINT ( 'NONE',  ( 0.1220691512310314308, 140.0123732041122935, 501.2786137957034498 ) ) ;
#18774 = DIRECTION ( 'NONE',  ( 0.000000000000000000, -1.000000000000000000, 0.000000000000000000 ) ) ;
#18775 = PRESENTATION_STYLE_ASSIGNMENT (( #7664 ) ) ;
#18776 = EDGE_CURVE ( 'NONE', #8466, #13536, #11286, .T. ) ;
#18777 = LINE ( 'NONE', #15512, #16941 ) ;
#18778 = EDGE_LOOP ( 'NONE', ( #9838, #3953, #12806, #2389 ) ) ;
#18779 = DIRECTION ( 'NONE',  ( 1.000000000000000000, -0.000000000000000000, 0.000000000000000000 ) ) ;
#18780 = CYLINDRICAL_SURFACE ( 'NONE', #17799, 4.000000000000000000 ) ;
#18781 = EDGE_LOOP ( 'NONE', ( #2281, #10925, #9499, #14367, #3329, #4708 ) ) ;
#18782 = DIRECTION ( 'NONE',  ( -1.000000000000000000, 0.000000000000000000, 1.450371633464475582E-15 ) ) ;
#18783 = ORIENTED_EDGE ( 'NONE', *, *, #1537, .T. ) ;
#18784 = EDGE_LOOP ( 'NONE', ( #19925, #10231, #19847, #1025 ) ) ;
#18785 = ORIENTED_EDGE ( 'NONE', *, *, #13493, .T. ) ;
#18786 = EDGE_CURVE ( 'NONE', #72, #16195, #1804, .T. ) ;
#18787 = COLOUR_RGB ( '', 0.31764706, 0.68627451, 0.89019608) ;
#18788 = EDGE_LOOP ( 'NONE', ( #13143, #16704, #10803, #20273, #15386 ) ) ;
#18789 =( NAMED_UNIT ( * ) PLANE_ANGLE_UNIT ( ) SI_UNIT ( $, .RADIAN. ) );
#18790 = EDGE_LOOP ( 'NONE', ( #485, #15469, #16857, #980 ) ) ;
#18791 =( LENGTH_UNIT ( ) NAMED_UNIT ( * ) SI_UNIT ( .MILLI., .METRE. ) );
#18792 = SURFACE_SIDE_STYLE ('',( #7582 ) ) ;
#18793 = DIRECTION ( 'NONE',  ( 0.000000000000000000, 0.000000000000000000, -1.000000000000000000 ) ) ;
#18795 = EDGE_CURVE ( 'NONE', #7705, #7373, #6261, .T. ) ;
#18794 = DIRECTION ( 'NONE',  ( 0.000000000000000000, 0.000000000000000000, -1.000000000000000000 ) ) ;
#18796 = SURFACE_STYLE_USAGE ( .BOTH. , #4811 ) ;
#18797 = EDGE_CURVE ( 'NONE', #18077, #8577, #12971, .T. ) ;
#18798 = ORIENTED_EDGE ( 'NONE', *, *, #9867, .F. ) ;
#18799 = DIRECTION ( 'NONE',  ( -1.000000000000000000, -1.595148023886719315E-16, 0.000000000000000000 ) ) ;
#18800 = SURFACE_SIDE_STYLE ('',( #12333 ) ) ;
#18801 = CIRCLE ( 'NONE', #2344, 4.000000000000003553 ) ;
#18802 = CARTESIAN_POINT ( 'NONE',  ( 53.48937290013659407, 0.000000000000000000, 250.0000000000000000 ) ) ;
#18803 = CARTESIAN_POINT ( 'NONE',  ( 463.8334540492693350, 191.8198460455371333, 178.2339398819846110 ) ) ;
#18804 = EDGE_CURVE ( 'NONE', #6007, #16512, #6361, .T. ) ;
#18805 = DIRECTION ( 'NONE',  ( 0.000000000000000000, 0.000000000000000000, 1.000000000000000000 ) ) ;
#18806 = ORIENTED_EDGE ( 'NONE', *, *, #7490, .F. ) ;
#18807 = EDGE_CURVE ( 'NONE', #14814, #9566, #5018, .T. ) ;
#18808 = EDGE_CURVE ( 'NONE', #7676, #15757, #5062, .T. ) ;
#18809 = ORIENTED_EDGE ( 'NONE', *, *, #7600, .T. ) ;
#18810 = VERTEX_POINT ( 'NONE', #3477 ) ;
#18811 = FILL_AREA_STYLE_COLOUR ( '', #15871 ) ;
#18812 = CARTESIAN_POINT ( 'NONE',  ( -81.00000000000133582, 139.4861549369088323, 500.2186618848270996 ) ) ;
#18813 = CIRCLE ( 'NONE', #8617, 3.300000000000011369 ) ;
#18814 = EDGE_LOOP ( 'NONE', ( #2340, #13333, #13804, #19173 ) ) ;
#18815 = CARTESIAN_POINT ( 'NONE',  ( 1.224646799147347044E-16, 38.00000000000000711, -0.9999999999999956701 ) ) ;
#18816 = PLANE ( 'NONE',  #2054 ) ;
#18817 = COLOUR_RGB ( '', 0.66274510, 0.83137255, 0.94901961) ;
#18818 = ORIENTED_EDGE ( 'NONE', *, *, #9011, .T. ) ;
#18819 = DIRECTION ( 'NONE',  ( -1.000000000000000000, 0.000000000000000000, -5.551115123125777653E-14 ) ) ;
#18820 = DIRECTION ( 'NONE',  ( -1.000000000000000000, -0.000000000000000000, -0.000000000000000000 ) ) ;
#18821 = EDGE_CURVE ( 'NONE', #8554, #12573, #9755, .T. ) ;
#18822 = DIRECTION ( 'NONE',  ( -6.123031769111888756E-17, 1.000000000000000000, 3.749151804555344967E-33 ) ) ;
#18823 = CIRCLE ( 'NONE', #713, 12.00000000000000178 ) ;
#18824 = DIRECTION ( 'NONE',  ( 0.000000000000000000, 0.000000000000000000, 1.000000000000000000 ) ) ;
#18825 = CARTESIAN_POINT ( 'NONE',  ( -31.00000000000000000, 11.00000000000000000, -31.00000000000000000 ) ) ;
#18826 = FILL_AREA_STYLE ('',( #6485 ) ) ;
#18827 = FACE_OUTER_BOUND ( 'NONE', #17966, .T. ) ;
#18828 = CARTESIAN_POINT ( 'NONE',  ( -1.000000000000015543, 147.7545334744432921, 491.0690926367356042 ) ) ;
#18829 = LINE ( 'NONE', #20283, #11211 ) ;
#18830 = VECTOR ( 'NONE', #17904, 1000.000000000000000 ) ;
#18831 = PRESENTATION_LAYER_ASSIGNMENT (  '', '', ( #11942 ) ) ;
#18832 =( GEOMETRIC_REPRESENTATION_CONTEXT ( 3 ) GLOBAL_UNCERTAINTY_ASSIGNED_CONTEXT ( ( #6493 ) ) GLOBAL_UNIT_ASSIGNED_CONTEXT ( ( #19627, #20341, #18994 ) ) REPRESENTATION_CONTEXT ( 'NONE', 'WORKASPACE' ) );
#18833 = ADVANCED_FACE ( 'NONE', ( #11598 ), #14892, .F. ) ;
#18834 = VERTEX_POINT ( 'NONE', #17684 ) ;
#18835 = ORIENTED_EDGE ( 'NONE', *, *, #4825, .T. ) ;
#18836 =( GEOMETRIC_REPRESENTATION_CONTEXT ( 3 ) GLOBAL_UNCERTAINTY_ASSIGNED_CONTEXT ( ( #13035 ) ) GLOBAL_UNIT_ASSIGNED_CONTEXT ( ( #11182, #20343, #12846 ) ) REPRESENTATION_CONTEXT ( 'NONE', 'WORKASPACE' ) );
#18837 = PLANE ( 'NONE',  #12009 ) ;
#18838 = EDGE_LOOP ( 'NONE', ( #20249, #15932, #9704, #12448, #13128 ) ) ;
#18839 = ORIENTED_EDGE ( 'NONE', *, *, #6015, .F. ) ;
#18840 = ORIENTED_EDGE ( 'NONE', *, *, #10, .T. ) ;
#18841 = DIRECTION ( 'NONE',  ( 0.000000000000000000, 0.000000000000000000, 1.000000000000000000 ) ) ;
#18842 = EDGE_CURVE ( 'NONE', #4572, #12596, #3573, .T. ) ;
#18843 = CARTESIAN_POINT ( 'NONE',  ( -79.99999999999995737, 216.7545334744432921, 489.5655098179848892 ) ) ;
#18844 = VECTOR ( 'NONE', #1863, 1000.000000000000000 ) ;
#18845 = STYLED_ITEM ( 'NONE', ( #3414 ), #18459 ) ;
#18846 = CARTESIAN_POINT ( 'NONE',  ( 0.000000000000000000, 138.7545334744432637, 0.000000000000000000 ) ) ;
#18847 = DIRECTION ( 'NONE',  ( 0.000000000000000000, 0.000000000000000000, -1.000000000000000000 ) ) ;
#18848 = SURFACE_STYLE_FILL_AREA ( #10829 ) ;
#18849 = PLANE ( 'NONE',  #6692 ) ;
#18850 = SURFACE_STYLE_FILL_AREA ( #9177 ) ;
#18851 = CARTESIAN_POINT ( 'NONE',  ( 3.000000000000000000, 1.836909530733565148E-16, 22.00000000000000000 ) ) ;
#18852 = LINE ( 'NONE', #20303, #420 ) ;
#18853 = ORIENTED_EDGE ( 'NONE', *, *, #16329, .T. ) ;
#18854 = EDGE_CURVE ( 'NONE', #6572, #13028, #11297, .T. ) ;
#18855 = AXIS2_PLACEMENT_3D ( 'NONE', #8856, #14010, #16714 ) ;
#18856 = CARTESIAN_POINT ( 'NONE',  ( 149.0892156028631348, 80.91625508013694912, 245.0000000000000000 ) ) ;
#18857 = LINE ( 'NONE', #7948, #18572 ) ;
#18858 = AXIS2_PLACEMENT_3D ( 'NONE', #6206, #4861, #17214 ) ;
#18859 = VECTOR ( 'NONE', #17465, 1000.000000000000000 ) ;
#18860 = ORIENTED_EDGE ( 'NONE', *, *, #5878, .T. ) ;
#18861 = MECHANICAL_DESIGN_GEOMETRIC_PRESENTATION_REPRESENTATION (  '', ( #14602 ), #13617 ) ;
#18862 = FACE_OUTER_BOUND ( 'NONE', #11107, .T. ) ;
#18863 = VECTOR ( 'NONE', #15585, 1000.000000000000000 ) ;
#18864 = ORIENTED_EDGE ( 'NONE', *, *, #4771, .T. ) ;
#18865 = FACE_OUTER_BOUND ( 'NONE', #12260, .T. ) ;
#18866 = ORIENTED_EDGE ( 'NONE', *, *, #3903, .T. ) ;
#18867 = VECTOR ( 'NONE', #16538, 1000.000000000000000 ) ;
#18868 = CARTESIAN_POINT ( 'NONE',  ( -81.18192946989275072, 138.7545334744432637, 500.8237260975782874 ) ) ;
#18869 = CARTESIAN_POINT ( 'NONE',  ( 36.99999999999999289, 10.00000000000000000, 22.99999999999999645 ) ) ;
#18870 = FILL_AREA_STYLE ('',( #18676 ) ) ;
#18871 = STYLED_ITEM ( 'NONE', ( #4575 ), #19037 ) ;
#18872 = VECTOR ( 'NONE', #6945, 1000.000000000000000 ) ;
#18873 = CARTESIAN_POINT ( 'NONE',  ( 0.2960399808010766298, 139.5465514659026667, 500.3567029293851647 ) ) ;
#18874 = CARTESIAN_POINT ( 'NONE',  ( -41.50085094405407915, 159.0821755739672483, 505.3921618609452935 ) ) ;
#18875 = DIRECTION ( 'NONE',  ( 1.000000000000000000, 0.000000000000000000, 0.000000000000000000 ) ) ;
#18876 = VECTOR ( 'NONE', #15388, 1000.000000000000000 ) ;
#18877 = CYLINDRICAL_SURFACE ( 'NONE', #1446, 9.999999999999998224 ) ;
#18878 = ORIENTED_EDGE ( 'NONE', *, *, #5591, .T. ) ;
#18879 = FACE_OUTER_BOUND ( 'NONE', #8913, .T. ) ;
#18880 = DIRECTION ( 'NONE',  ( -1.000000000000000000, 0.000000000000000000, 0.000000000000000000 ) ) ;
#18881 = CONTEXT_DEPENDENT_SHAPE_REPRESENTATION ( #3156, #14366 ) ;
#18882 = CIRCLE ( 'NONE', #9007, 4.999999999999997335 ) ;
#18883 = EDGE_LOOP ( 'NONE', ( #10856, #7163, #1669, #6875 ) ) ;
#18884 = EDGE_LOOP ( 'NONE', ( #2804, #17098, #7281, #11527 ) ) ;
#18885 = VECTOR ( 'NONE', #19353, 1000.000000000000000 ) ;
#18886 = DIRECTION ( 'NONE',  ( 9.815121534730717399E-17, -1.000000000000000000, 0.000000000000000000 ) ) ;
#18887 = EDGE_LOOP ( 'NONE', ( #244, #7179, #13088, #20072 ) ) ;
#18888 = VECTOR ( 'NONE', #8944, 1000.000000000000000 ) ;
#18889 = ORIENTED_EDGE ( 'NONE', *, *, #15809, .F. ) ;
#18890 = EDGE_CURVE ( 'NONE', #17942, #4680, #7077, .T. ) ;
#18891 = ORIENTED_EDGE ( 'NONE', *, *, #3732, .F. ) ;
#18892 = VECTOR ( 'NONE', #9332, 1000.000000000000000 ) ;
#18893 = AXIS2_PLACEMENT_3D ( 'NONE', #11763, #993, #5666 ) ;
#18894 = PRESENTATION_LAYER_ASSIGNMENT (  '', '', ( #19241 ) ) ;
#18895 = CARTESIAN_POINT ( 'NONE',  ( 22.99999999999998224, 6.000000000000000000, -31.99999999999998579 ) ) ;
#18896 = CONICAL_SURFACE ( 'NONE', #8389, 12.32407335584850117, 0.8899833664651138898 ) ;
#18897 = ORIENTED_EDGE ( 'NONE', *, *, #17469, .T. ) ;
#18898 = DIRECTION ( 'NONE',  ( 0.000000000000000000, -0.000000000000000000, -1.000000000000000000 ) ) ;
#18899 =( NAMED_UNIT ( * ) SI_UNIT ( $, .STERADIAN. ) SOLID_ANGLE_UNIT ( ) );
#18900 = ORIENTED_EDGE ( 'NONE', *, *, #13574, .T. ) ;
#18901 = SURFACE_SIDE_STYLE ('',( #6248 ) ) ;
#18902 = FACE_OUTER_BOUND ( 'NONE', #6195, .T. ) ;
#18903 = PRESENTATION_LAYER_ASSIGNMENT (  '', '', ( #8712 ) ) ;
#18904 = SURFACE_STYLE_FILL_AREA ( #17564 ) ;
#18905 = AXIS2_PLACEMENT_3D ( 'NONE', #4724, #11014, #13280 ) ;
#18906 = DIRECTION ( 'NONE',  ( 1.000000000000000000, 0.000000000000000000, 0.000000000000000000 ) ) ;
#18907 = CARTESIAN_POINT ( 'NONE',  ( 19.99999999999995381, 3.000000000000000000, -36.99999999999999289 ) ) ;
#18908 = DIRECTION ( 'NONE',  ( 1.000000000000000000, -0.000000000000000000, -0.000000000000000000 ) ) ;
#18909 = DIRECTION ( 'NONE',  ( 0.000000000000000000, 1.000000000000000000, 0.000000000000000000 ) ) ;
#18910 = ORIENTED_EDGE ( 'NONE', *, *, #10472, .F. ) ;
#18911 = ADVANCED_FACE ( 'NONE', ( #8716 ), #16370, .T. ) ;
#18912 = CIRCLE ( 'NONE', #10044, 10.00000000000000888 ) ;
#18913 = CARTESIAN_POINT ( 'NONE',  ( 35.00000000000003553, 3.000000000000000000, -20.99999999999999645 ) ) ;
#18914 = CARTESIAN_POINT ( 'NONE',  ( -31.81980515339462912, 8.000000000000000000, 31.81980515339465043 ) ) ;
#18915 = LINE ( 'NONE', #6263, #4450 ) ;
#18916 = DIRECTION ( 'NONE',  ( 0.000000000000000000, -0.000000000000000000, -1.000000000000000000 ) ) ;
#18917 = ORIENTED_EDGE ( 'NONE', *, *, #1034, .T. ) ;
#18918 = VECTOR ( 'NONE', #8008, 1000.000000000000000 ) ;
#18919 = STYLED_ITEM ( 'NONE', ( #16359 ), #1227 ) ;
#18920 = ORIENTED_EDGE ( 'NONE', *, *, #16533, .T. ) ;
#18921 = AXIS2_PLACEMENT_3D ( 'NONE', #13860, #1155, #5928 ) ;
#18922 = EDGE_CURVE ( 'NONE', #16181, #17991, #17983, .T. ) ;
#18923 = VERTEX_POINT ( 'NONE', #16455 ) ;
#18924 = SURFACE_SIDE_STYLE ('',( #9547 ) ) ;
#18925 = CARTESIAN_POINT ( 'NONE',  ( -80.17963259596821501, 139.9670406124139674, 501.2044833972698825 ) ) ;
#18926 = ORIENTED_EDGE ( 'NONE', *, *, #1002, .T. ) ;
#18927 = SURFACE_STYLE_FILL_AREA ( #17290 ) ;
#18928 = FILL_AREA_STYLE ('',( #12664 ) ) ;
#18929 = ADVANCED_FACE ( 'NONE', ( #2303 ), #8597, .F. ) ;
#18930 = VERTEX_POINT ( 'NONE', #9203 ) ;
#18931 = DIRECTION ( 'NONE',  ( -1.000000000000000000, -0.000000000000000000, -0.000000000000000000 ) ) ;
#18932 = VECTOR ( 'NONE', #228, 1000.000000000000000 ) ;
#18933 = PLANE ( 'NONE',  #8415 ) ;
#18934 = CARTESIAN_POINT ( 'NONE',  ( -2.383743612111324239, 61.83195493428745237, 9.196765735797573171 ) ) ;
#18935 = DIRECTION ( 'NONE',  ( 0.000000000000000000, 0.000000000000000000, -1.000000000000000000 ) ) ;
#18936 = AXIS2_PLACEMENT_3D ( 'NONE', #3556, #14769, #4152 ) ;
#18937 = DIRECTION ( 'NONE',  ( 1.000000000000000000, 0.000000000000000000, 0.000000000000000000 ) ) ;
#18938 = PLANE ( 'NONE',  #4952 ) ;
#18939 = ADVANCED_FACE ( 'NONE', ( #13750, #13655 ), #5918, .F. ) ;
#18940 = DIRECTION ( 'NONE',  ( 1.000000000000000000, 0.000000000000000000, 0.000000000000000000 ) ) ;
#18941 = CARTESIAN_POINT ( 'NONE',  ( 40.00000000000001421, 3.000000000000000888, -150.0000000000000000 ) ) ;
#18942 = DIRECTION ( 'NONE',  ( 0.000000000000000000, 1.000000000000000000, 0.000000000000000000 ) ) ;
#18943 = EDGE_CURVE ( 'NONE', #6958, #12894, #3070, .T. ) ;
#18944 = ORIENTED_EDGE ( 'NONE', *, *, #16709, .F. ) ;
#18945 = VERTEX_POINT ( 'NONE', #4187 ) ;
#18946 = EDGE_CURVE ( 'NONE', #13149, #16512, #15195, .T. ) ;
#18947 = ORIENTED_EDGE ( 'NONE', *, *, #15326, .F. ) ;
#18948 = ORIENTED_EDGE ( 'NONE', *, *, #9618, .F. ) ;
#18949 = EDGE_LOOP ( 'NONE', ( #2201, #19686, #2233, #10933 ) ) ;
#18950 = CARTESIAN_POINT ( 'NONE',  ( 35.99999999999999289, 10.00000000000000000, 17.99999999999998934 ) ) ;
#18951 = AXIS2_PLACEMENT_3D ( 'NONE', #12576, #1302, #18841 ) ;
#18952 =( NAMED_UNIT ( * ) PLANE_ANGLE_UNIT ( ) SI_UNIT ( $, .RADIAN. ) );
#18953 = CARTESIAN_POINT ( 'NONE',  ( 4.899999999999999467, 0.000000000000000000, 0.000000000000000000 ) ) ;
#18954 = FACE_OUTER_BOUND ( 'NONE', #12445, .T. ) ;
#18955 = DIRECTION ( 'NONE',  ( -1.000000000000000000, 0.000000000000000000, 0.000000000000000000 ) ) ;
#18956 = EDGE_CURVE ( 'NONE', #13165, #8469, #15263, .T. ) ;
#18957 =( GEOMETRIC_REPRESENTATION_CONTEXT ( 3 ) GLOBAL_UNCERTAINTY_ASSIGNED_CONTEXT ( ( #19581 ) ) GLOBAL_UNIT_ASSIGNED_CONTEXT ( ( #4229, #899, #4133 ) ) REPRESENTATION_CONTEXT ( 'NONE', 'WORKASPACE' ) );
#18958 = PRODUCT ( 'Part4', 'Part4', '', ( #18590 ) ) ;
#18959 = VERTEX_POINT ( 'NONE', #19704 ) ;
#18960 = DIRECTION ( 'NONE',  ( 0.000000000000000000, 0.000000000000000000, 1.000000000000000000 ) ) ;
#18961 = LINE ( 'NONE', #1626, #1529 ) ;
#18962 = DIRECTION ( 'NONE',  ( -3.854941057726255847E-16, -0.000000000000000000, 1.000000000000000000 ) ) ;
#18963 = CARTESIAN_POINT ( 'NONE',  ( -34.99999999999996447, 8.000000000000000000, -40.00000000000000711 ) ) ;
#18964 = ORIENTED_EDGE ( 'NONE', *, *, #4327, .T. ) ;
#18965 = SURFACE_SIDE_STYLE ('',( #14041 ) ) ;
#18966 = ORIENTED_EDGE ( 'NONE', *, *, #16427, .T. ) ;
#18967 = EDGE_LOOP ( 'NONE', ( #14370, #5345, #17256, #1466 ) ) ;
#18968 = EDGE_CURVE ( 'NONE', #16895, #7678, #6387, .T. ) ;
#18969 = DIRECTION ( 'NONE',  ( 0.000000000000000000, 0.000000000000000000, 1.000000000000000000 ) ) ;
#18970 = ORIENTED_EDGE ( 'NONE', *, *, #8382, .F. ) ;
#18971 = LINE ( 'NONE', #14446, #4458 ) ;
#18972 = CARTESIAN_POINT ( 'NONE',  ( -31.00000000000002132, 10.00000000000000000, -31.00000000000000000 ) ) ;
#18973 = LINE ( 'NONE', #24, #4432 ) ;
#18974 = ADVANCED_FACE ( 'NONE', ( #4075 ), #1042, .F. ) ;
#18975 = CARTESIAN_POINT ( 'NONE',  ( -0.1029799530868260177, 140.5738215973348701, 502.0971144060484335 ) ) ;
#18976 = DIRECTION ( 'NONE',  ( 0.000000000000000000, 0.000000000000000000, -1.000000000000000000 ) ) ;
#18977 = CARTESIAN_POINT ( 'NONE',  ( 31.00000000000004263, 68.00000000000000000, -25.99999999999999645 ) ) ;
#18978 = DIRECTION ( 'NONE',  ( 6.123031769111888756E-17, -1.000000000000000000, -3.749151804555344967E-33 ) ) ;
#18979 = ORIENTED_EDGE ( 'NONE', *, *, #11946, .F. ) ;
#18980 = DIRECTION ( 'NONE',  ( -0.000000000000000000, -1.000000000000000000, -0.000000000000000000 ) ) ;
#18981 = DIRECTION ( 'NONE',  ( -0.000000000000000000, 1.000000000000000000, -0.000000000000000000 ) ) ;
#18982 = CARTESIAN_POINT ( 'NONE',  ( -26.00000000000002132, 0.000000000000000000, -31.00000000000003553 ) ) ;
#18983 = ORIENTED_EDGE ( 'NONE', *, *, #20178, .T. ) ;
#18985 = ORIENTED_EDGE ( 'NONE', *, *, #15171, .F. ) ;
#18984 = AXIS2_PLACEMENT_3D ( 'NONE', #10105, #13415, #19456 ) ;
#18986 = DIRECTION ( 'NONE',  ( 0.000000000000000000, 0.000000000000000000, -1.000000000000000000 ) ) ;
#18987 = ORIENTED_EDGE ( 'NONE', *, *, #549, .T. ) ;
#18988 = ORIENTED_EDGE ( 'NONE', *, *, #14694, .F. ) ;
#18989 = EDGE_LOOP ( 'NONE', ( #16954, #5143, #4400, #2923 ) ) ;
#18990 = DIRECTION ( 'NONE',  ( 0.000000000000000000, 0.000000000000000000, -1.000000000000000000 ) ) ;
#18991 = ORIENTED_EDGE ( 'NONE', *, *, #8429, .T. ) ;
#18992 =( GEOMETRIC_REPRESENTATION_CONTEXT ( 3 ) GLOBAL_UNCERTAINTY_ASSIGNED_CONTEXT ( ( #3193 ) ) GLOBAL_UNIT_ASSIGNED_CONTEXT ( ( #8681, #18042, #8480 ) ) REPRESENTATION_CONTEXT ( 'NONE', 'WORKASPACE' ) );
#18993 = FACE_OUTER_BOUND ( 'NONE', #18790, .T. ) ;
#18994 =( NAMED_UNIT ( * ) SI_UNIT ( $, .STERADIAN. ) SOLID_ANGLE_UNIT ( ) );
#18995 = AXIS2_PLACEMENT_3D ( 'NONE', #5154, #5041, #15991 ) ;
#18996 = CARTESIAN_POINT ( 'NONE',  ( -75.00000000000000000, 313.8311070602663904, -87.78239810828596035 ) ) ;
#18997 = CARTESIAN_POINT ( 'NONE',  ( -81.00000000000127898, 139.7703989349477354, 489.5655098179835818 ) ) ;
#18998 = PRESENTATION_STYLE_ASSIGNMENT (( #18796 ) ) ;
#18999 = EDGE_CURVE ( 'NONE', #36, #11766, #14264, .T. ) ;
#19000 = CARTESIAN_POINT ( 'NONE',  ( -0.9699764831012689381, 38.15427877784792088, 9.452135968713491820 ) ) ;
#19001 = ORIENTED_EDGE ( 'NONE', *, *, #10506, .F. ) ;
#19002 = CARTESIAN_POINT ( 'NONE',  ( -18.00000000000001421, 10.00000000000000000, 37.00000000000000711 ) ) ;
#19003 = CARTESIAN_POINT ( 'NONE',  ( 0.000000000000000000, 0.000000000000000000, 0.000000000000000000 ) ) ;
#19004 = LINE ( 'NONE', #4910, #1765 ) ;
#19005 = FACE_OUTER_BOUND ( 'NONE', #19502, .T. ) ;
#19006 = DIRECTION ( 'NONE',  ( 1.000000000000000000, -0.000000000000000000, 0.000000000000000000 ) ) ;
#19007 = CARTESIAN_POINT ( 'NONE',  ( 53.48937290013658696, 122.8810204491430369, 322.0399576098686225 ) ) ;
#19008 = ORIENTED_EDGE ( 'NONE', *, *, #10008, .T. ) ;
#19009 = CIRCLE ( 'NONE', #20337, 10.00000000000000888 ) ;
#19010 = VERTEX_POINT ( 'NONE', #19810 ) ;
#19011 = DIRECTION ( 'NONE',  ( -0.000000000000000000, -1.000000000000000000, 0.000000000000000000 ) ) ;
#19012 = DIRECTION ( 'NONE',  ( 0.000000000000000000, 0.000000000000000000, 1.000000000000000000 ) ) ;
#19013 = ADVANCED_FACE ( 'NONE', ( #12016 ), #2819, .F. ) ;
#19014 = EDGE_LOOP ( 'NONE', ( #936, #1839, #18536, #18231 ) ) ;
#19015 = DIRECTION ( 'NONE',  ( 1.000000000000000000, 9.815121534730718631E-17, 0.000000000000000000 ) ) ;
#19016 = CYLINDRICAL_SURFACE ( 'NONE', #9957, 3.283624802691453848 ) ;
#19017 = ORIENTED_EDGE ( 'NONE', *, *, #15437, .F. ) ;
#19018 = FACE_OUTER_BOUND ( 'NONE', #16517, .T. ) ;
#19019 = LINE ( 'NONE', #12558, #18591 ) ;
#19020 = CARTESIAN_POINT ( 'NONE',  ( 40.00000000000001421, -5.000000000000000888, 0.000000000000000000 ) ) ;
#19021 = CARTESIAN_POINT ( 'NONE',  ( 423.8334540492694487, 191.8198460455371333, 235.0057801310552463 ) ) ;
#19022 = PLANE ( 'NONE',  #1388 ) ;
#19023 = LINE ( 'NONE', #17302, #3648 ) ;
#19024 = DIRECTION ( 'NONE',  ( 0.000000000000000000, 0.000000000000000000, 1.000000000000000000 ) ) ;
#19025 = EDGE_CURVE ( 'NONE', #658, #19735, #4368, .T. ) ;
#19026 = DIRECTION ( 'NONE',  ( 0.000000000000000000, 0.000000000000000000, 1.000000000000000000 ) ) ;
#19027 = CARTESIAN_POINT ( 'NONE',  ( -81.18192946989242387, 139.7703989349477354, 490.5655098180907885 ) ) ;
#19028 = ORIENTED_EDGE ( 'NONE', *, *, #2560, .F. ) ;
#19029 = PRODUCT_RELATED_PRODUCT_CATEGORY ( 'part', '', ( #12546 ) ) ;
#19030 = ORIENTED_EDGE ( 'NONE', *, *, #5218, .T. ) ;
#19031 = ORIENTED_EDGE ( 'NONE', *, *, #17492, .F. ) ;
#19032 = UNCERTAINTY_MEASURE_WITH_UNIT (LENGTH_MEASURE( 1.000000000000000082E-05 ), #13935, 'distance_accuracy_value', 'NONE');
#19033 = AXIS2_PLACEMENT_3D ( 'NONE', #11837, #968, #3696 ) ;
#19034 = CARTESIAN_POINT ( 'NONE',  ( 25.99999999999998224, 0.000000000000000000, -31.00000000000003197 ) ) ;
#19035 = AXIS2_PLACEMENT_3D ( 'NONE', #8418, #5515, #11805 ) ;
#19036 = VERTEX_POINT ( 'NONE', #15308 ) ;
#19037 = ADVANCED_FACE ( 'NONE', ( #10653 ), #15408, .F. ) ;
#19038 = VERTEX_POINT ( 'NONE', #17248 ) ;
#19039 = CARTESIAN_POINT ( 'NONE',  ( -79.99999999999995737, 316.7545334744432353, 495.1946179577816451 ) ) ;
#19040 =( LENGTH_UNIT ( ) NAMED_UNIT ( * ) SI_UNIT ( .MILLI., .METRE. ) );
#19041 = SURFACE_SIDE_STYLE ('',( #9686 ) ) ;
#19042 = ADVANCED_FACE ( 'NONE', ( #9604 ), #4885, .F. ) ;
#19043 = DIRECTION ( 'NONE',  ( 0.000000000000000000, 1.000000000000000000, 0.000000000000000000 ) ) ;
#19044 = DIRECTION ( 'NONE',  ( -0.000000000000000000, -1.000000000000000000, -0.000000000000000000 ) ) ;
#19045 = FACE_OUTER_BOUND ( 'NONE', #3754, .T. ) ;
#19046 = DIRECTION ( 'NONE',  ( 1.000000000000000000, 0.000000000000000000, 0.000000000000000000 ) ) ;
#19047 = VECTOR ( 'NONE', #4534, 1000.000000000000000 ) ;
#19048 =( LENGTH_UNIT ( ) NAMED_UNIT ( * ) SI_UNIT ( .MILLI., .METRE. ) );
#19049 = AXIS2_PLACEMENT_3D ( 'NONE', #8157, #8045, #14333 ) ;
#19050 = CARTESIAN_POINT ( 'NONE',  ( 40.00000000000000000, 68.00000000000000000, 26.00000000000000355 ) ) ;
#19051 = DIRECTION ( 'NONE',  ( -0.000000000000000000, -0.000000000000000000, 1.000000000000000000 ) ) ;
#19052 = ADVANCED_FACE ( 'NONE', ( #4674 ), #3139, .F. ) ;
#19053 = COLOUR_RGB ( '', 0.72549020, 0.75294118, 0.79215686) ;
#19054 = ORIENTED_EDGE ( 'NONE', *, *, #18703, .T. ) ;
#19055 = VECTOR ( 'NONE', #18612, 1000.000000000000000 ) ;
#19056 = DIRECTION ( 'NONE',  ( 1.000000000000000000, 0.000000000000000000, -0.000000000000000000 ) ) ;
#19057 = EDGE_CURVE ( 'NONE', #16598, #11036, #6233, .T. ) ;
#19058 = EDGE_CURVE ( 'NONE', #9818, #4114, #6403, .T. ) ;
#19059 = EDGE_LOOP ( 'NONE', ( #8321, #2047, #14728, #333 ) ) ;
#19060 = DIRECTION ( 'NONE',  ( -7.900838015626929923E-17, -8.586860021784410058E-33, 1.000000000000000000 ) ) ;
#19061 = VERTEX_POINT ( 'NONE', #1770 ) ;
#19062 = MECHANICAL_DESIGN_GEOMETRIC_PRESENTATION_REPRESENTATION (  '', ( #11857 ), #10522 ) ;
#19063 = ADVANCED_FACE ( 'NONE', ( #6442 ), #9729, .T. ) ;
#19064 = PRESENTATION_LAYER_ASSIGNMENT (  '', '', ( #20044 ) ) ;
#19065 = VECTOR ( 'NONE', #12405, 1000.000000000000000 ) ;
#19066 = SURFACE_STYLE_FILL_AREA ( #12713 ) ;
#19067 = ORIENTED_EDGE ( 'NONE', *, *, #1672, .T. ) ;
#19068 = EDGE_CURVE ( 'NONE', #19948, #9269, #13955, .T. ) ;
#19069 = CARTESIAN_POINT ( 'NONE',  ( -40.00000000000000000, 68.00000000000000000, 26.00000000000000355 ) ) ;
#19070 = DIRECTION ( 'NONE',  ( -0.000000000000000000, -0.7071067811865614505, -0.7071067811865336949 ) ) ;
#19071 = VERTEX_POINT ( 'NONE', #18982 ) ;
#19072 = LINE ( 'NONE', #17530, #18603 ) ;
#19073 = CARTESIAN_POINT ( 'NONE',  ( 31.00000000000006750, 19.00000000000000000, -21.00000000000000355 ) ) ;
#19074 = DIRECTION ( 'NONE',  ( 0.000000000000000000, 0.7071067811865336949, -0.7071067811865614505 ) ) ;
#19075 = CARTESIAN_POINT ( 'NONE',  ( -1.214306433183764808E-14, 140.8764026050585301, 502.4686618848270996 ) ) ;
#19076 = DIRECTION ( 'NONE',  ( -0.000000000000000000, -1.000000000000000000, 0.000000000000000000 ) ) ;
#19077 = CARTESIAN_POINT ( 'NONE',  ( -79.99999999999995737, 140.1563709946295262, 488.5655098179835818 ) ) ;
#19078 = CARTESIAN_POINT ( 'NONE',  ( -75.00000000000000000, 313.8311070602663904, -87.78239810828596035 ) ) ;
#19079 = EDGE_CURVE ( 'NONE', #14963, #16910, #8085, .T. ) ;
#19080 = ORIENTED_EDGE ( 'NONE', *, *, #17038, .F. ) ;
#19081 = CYLINDRICAL_SURFACE ( 'NONE', #9491, 3.300000000000025135 ) ;
#19082 = CARTESIAN_POINT ( 'NONE',  ( 493.8117674897343363, 134.2156642432025251, 245.0000000000000000 ) ) ;
#19083 =( GEOMETRIC_REPRESENTATION_CONTEXT ( 3 ) GLOBAL_UNCERTAINTY_ASSIGNED_CONTEXT ( ( #16122 ) ) GLOBAL_UNIT_ASSIGNED_CONTEXT ( ( #5616, #18165, #17982 ) ) REPRESENTATION_CONTEXT ( 'NONE', 'WORKASPACE' ) );
#19084 = APPLICATION_PROTOCOL_DEFINITION ( 'draft international standard', 'automotive_design', 1998, #3552 ) ;
#19085 = CIRCLE ( 'NONE', #10876, 9.500000000000000000 ) ;
#19086 = CIRCLE ( 'NONE', #15117, 5.000000000000004441 ) ;
#19087 = ORIENTED_EDGE ( 'NONE', *, *, #19187, .F. ) ;
#19088 = LINE ( 'NONE', #3652, #12234 ) ;
#19089 = ORIENTED_EDGE ( 'NONE', *, *, #7319, .T. ) ;
#19090 = VERTEX_POINT ( 'NONE', #12827 ) ;
#19091 = ORIENTED_EDGE ( 'NONE', *, *, #7710, .T. ) ;
#19092 = ADVANCED_FACE ( 'NONE', ( #20235 ), #7672, .F. ) ;
#19093 = DIRECTION ( 'NONE',  ( 0.000000000000000000, 0.000000000000000000, 1.000000000000000000 ) ) ;
#19094 = B_SPLINE_CURVE_WITH_KNOTS ( 'NONE', 3,
 ( #452, #12953, #350, #5116, #9741, #17672, #3561, #5213, #14773, #16253 ),
 .UNSPECIFIED., .F., .F.,
 ( 4, 2, 2, 2, 4 ),
 ( 0.000000000000000000, 0.0004090546821513940776, 0.0008181093643027881552, 0.001227164046454182287, 0.001636218728605576310 ),
 .UNSPECIFIED. ) ;
#19095 = ADVANCED_FACE ( 'NONE', ( #1558 ), #12419, .F. ) ;
#19096 = CARTESIAN_POINT ( 'NONE',  ( 1.050000000000000044, 0.000000000000000000, 0.000000000000000000 ) ) ;
#19097 = ORIENTED_EDGE ( 'NONE', *, *, #791, .T. ) ;
#19098 = DIRECTION ( 'NONE',  ( -6.123031769111888756E-17, 1.000000000000000000, 3.749151804555344967E-33 ) ) ;
#19099 = VECTOR ( 'NONE', #2472, 1000.000000000000000 ) ;
#19100 = ADVANCED_FACE ( 'NONE', ( #5203 ), #13236, .F. ) ;
#19101 = PRESENTATION_STYLE_ASSIGNMENT (( #12627 ) ) ;
#19102 = EDGE_LOOP ( 'NONE', ( #2807, #14069, #18696, #4280 ) ) ;
#19103 = PRESENTATION_LAYER_ASSIGNMENT (  '', '', ( #15839 ) ) ;
#19104 = FACE_OUTER_BOUND ( 'NONE', #4745, .T. ) ;
#19105 = COLOUR_RGB ( '', 0.31764706, 0.68627451, 0.89019608) ;
#19106 = CARTESIAN_POINT ( 'NONE',  ( -37.00000000000000000, 0.000000000000000000, -22.99999999999999645 ) ) ;
#19107 = DIRECTION ( 'NONE',  ( -1.000000000000000000, -9.815121534730717399E-17, 0.000000000000000000 ) ) ;
#19108 = DIRECTION ( 'NONE',  ( 0.000000000000000000, 0.000000000000000000, -1.000000000000000000 ) ) ;
#19109 = DIRECTION ( 'NONE',  ( -0.000000000000000000, -1.000000000000000000, -0.000000000000000000 ) ) ;
#19110 = ORIENTED_EDGE ( 'NONE', *, *, #8631, .T. ) ;
#19111 = CARTESIAN_POINT ( 'NONE',  ( 30.99999999999997513, 10.00000000000000000, 30.99999999999999645 ) ) ;
#19112 = LINE ( 'NONE', #15849, #11895 ) ;
#19113 = DIRECTION ( 'NONE',  ( 0.000000000000000000, -1.000000000000000000, 0.000000000000000000 ) ) ;
#19114 = CARTESIAN_POINT ( 'NONE',  ( 1.836909530733565148E-16, 0.000000000000000000, 3.000000000000000000 ) ) ;
#19115 = VERTEX_POINT ( 'NONE', #1872 ) ;
#19116 = CYLINDRICAL_SURFACE ( 'NONE', #12911, 3.000000000000016431 ) ;
#19117 = LINE ( 'NONE', #17781, #3946 ) ;
#19118 = VECTOR ( 'NONE', #3360, 1000.000000000000000 ) ;
#19119 = EDGE_LOOP ( 'NONE', ( #20122, #8537, #12735, #1152 ) ) ;
#19120 = VECTOR ( 'NONE', #3807, 1000.000000000000000 ) ;
#19121 =( GEOMETRIC_REPRESENTATION_CONTEXT ( 3 ) GLOBAL_UNCERTAINTY_ASSIGNED_CONTEXT ( ( #11995 ) ) GLOBAL_UNIT_ASSIGNED_CONTEXT ( ( #6608, #14028, #9387 ) ) REPRESENTATION_CONTEXT ( 'NONE', 'WORKASPACE' ) );
#19122 = ORIENTED_EDGE ( 'NONE', *, *, #2801, .T. ) ;
#19123 = B_SPLINE_CURVE_WITH_KNOTS ( 'NONE', 3,
 ( #1981, #6774, #556, #13065, #16357, #14688, #5311, #2285, #6867, #13151, #17867, #3764, #2192, #647, #6960, #13243 ),
 .UNSPECIFIED., .F., .F.,
 ( 4, 2, 2, 2, 2, 2, 2, 4 ),
 ( 0.000000000000000000, 0.0005901654530283999755, 0.001180330906056799951, 0.001770496359085199818, 0.002360661812113599902, 0.003540992718170399636, 0.004131158171198803623, 0.004721323624227206743 ),
 .UNSPECIFIED. ) ;
#19124 = EDGE_CURVE ( 'NONE', #10668, #4192, #4085, .T. ) ;
#19125 = VERTEX_POINT ( 'NONE', #11474 ) ;
#19126 = CARTESIAN_POINT ( 'NONE',  ( -80.31210361190693447, 139.8880426697628820, 501.0724697727050057 ) ) ;
#19127 = ORIENTED_EDGE ( 'NONE', *, *, #12887, .F. ) ;
#19128 = DIRECTION ( 'NONE',  ( 1.000000000000000000, 0.000000000000000000, -0.000000000000000000 ) ) ;
#19129 = VERTEX_POINT ( 'NONE', #14459 ) ;
#19130 = CARTESIAN_POINT ( 'NONE',  ( 111.4893729001366012, 125.7247684487574588, 254.0000000000000000 ) ) ;
#19131 = CIRCLE ( 'NONE', #17829, 3.999999999999996447 ) ;
#19132 = CARTESIAN_POINT ( 'NONE',  ( -1.274252908074454287E-14, 140.1563709946295262, 488.5655098179835818 ) ) ;
#19133 = CYLINDRICAL_SURFACE ( 'NONE', #764, 3.300000000000011369 ) ;
#19134 = AXIS2_PLACEMENT_3D ( 'NONE', #4463, #18183, #15015 ) ;
#19135 = CARTESIAN_POINT ( 'NONE',  ( 10.00000000000000000, 341.0487089519837696, -96.50000000000331113 ) ) ;
#19136 = CARTESIAN_POINT ( 'NONE',  ( 3.674999999999999822, 0.000000000000000000, 0.000000000000000000 ) ) ;
#19137 = CARTESIAN_POINT ( 'NONE',  ( 503.8334540492693918, 191.8198460455371333, 81.76606011801540319 ) ) ;
#19138 = DIRECTION ( 'NONE',  ( 0.000000000000000000, -1.000000000000000000, 0.000000000000000000 ) ) ;
#19139 = CARTESIAN_POINT ( 'NONE',  ( 153.4893729001366580, 80.91625508013694912, 0.000000000000000000 ) ) ;
#19140 = SURFACE_STYLE_USAGE ( .BOTH. , #17806 ) ;
#19141 = ORIENTED_EDGE ( 'NONE', *, *, #14401, .F. ) ;
#19142 = ORIENTED_EDGE ( 'NONE', *, *, #5575, .T. ) ;
#19143 = CIRCLE ( 'NONE', #6339, 9.000000000000007105 ) ;
#19144 = VERTEX_POINT ( 'NONE', #14675 ) ;
#19145 = EDGE_CURVE ( 'NONE', #11813, #2874, #7702, .T. ) ;
#19146 = DIRECTION ( 'NONE',  ( 0.000000000000000000, 0.000000000000000000, -1.000000000000000000 ) ) ;
#19147 = STYLED_ITEM ( 'NONE', ( #5843 ), #8197 ) ;
#19148 = ORIENTED_EDGE ( 'NONE', *, *, #12594, .T. ) ;
#19149 = VERTEX_POINT ( 'NONE', #638 ) ;
#19150 = ORIENTED_EDGE ( 'NONE', *, *, #9406, .T. ) ;
#19151 = CARTESIAN_POINT ( 'NONE',  ( 1.399999999999999911, -13.62500000000000000, -1.668581263838268760E-15 ) ) ;
#19152 = LINE ( 'NONE', #301, #13331 ) ;
#19153 =( GEOMETRIC_REPRESENTATION_CONTEXT ( 3 ) GLOBAL_UNCERTAINTY_ASSIGNED_CONTEXT ( ( #5549 ) ) GLOBAL_UNIT_ASSIGNED_CONTEXT ( ( #5019, #7696, #14178 ) ) REPRESENTATION_CONTEXT ( 'NONE', 'WORKASPACE' ) );
#19154 = CARTESIAN_POINT ( 'NONE',  ( -20.00000000000003197, 0.000000000000000000, 40.00000000000000711 ) ) ;
#19155 = FILL_AREA_STYLE_COLOUR ( '', #9863 ) ;
#19156 = DIRECTION ( 'NONE',  ( 0.000000000000000000, 0.000000000000000000, -1.000000000000000000 ) ) ;
#19157 = DIRECTION ( 'NONE',  ( 0.000000000000000000, 0.7071067811865504593, -0.7071067811865445751 ) ) ;
#19158 =( NAMED_UNIT ( * ) SI_UNIT ( $, .STERADIAN. ) SOLID_ANGLE_UNIT ( ) );
#19159 = AXIS2_PLACEMENT_3D ( 'NONE', #19412, #14888, #7075 ) ;
#19160 = CARTESIAN_POINT ( 'NONE',  ( -39.99999999999997868, 3.000000000000000000, 26.00000000000000355 ) ) ;
#19161 = AXIS2_PLACEMENT_3D ( 'NONE', #4842, #19024, #12563 ) ;
#19162 = AXIS2_PLACEMENT_3D ( 'NONE', #16369, #3361, #2104 ) ;
#19163 = PLANE ( 'NONE',  #15970 ) ;
#19164 = CYLINDRICAL_SURFACE ( 'NONE', #17460, 10.00000000000001066 ) ;
#19165 = CARTESIAN_POINT ( 'NONE',  ( 0.000000000000000000, 66.00000000000000000, -9.500000000000000000 ) ) ;
#19166 = COLOUR_RGB ( '', 0.66274510, 0.83137255, 0.94901961) ;
#19167 =( NAMED_UNIT ( * ) SI_UNIT ( $, .STERADIAN. ) SOLID_ANGLE_UNIT ( ) );
#19168 = EDGE_CURVE ( 'NONE', #1696, #6058, #3647, .T. ) ;
#19169 = CARTESIAN_POINT ( 'NONE',  ( 2.181929469892510465, 139.7703989349544145, 490.5655098179848324 ) ) ;
#19170 = COLOUR_RGB ( '', 0.40784314, 0.44705882, 0.49803922) ;
#19171 = ORIENTED_EDGE ( 'NONE', *, *, #574, .F. ) ;
#19172 = CARTESIAN_POINT ( 'NONE',  ( 31.00000000000000000, 19.00000000000000000, -21.00000000000000355 ) ) ;
#19173 = ORIENTED_EDGE ( 'NONE', *, *, #2707, .T. ) ;
#19174 = VECTOR ( 'NONE', #14083, 1000.000000000000000 ) ;
#19175 = CIRCLE ( 'NONE', #1378, 10.00000000000000888 ) ;
#19176 = AXIS2_PLACEMENT_3D ( 'NONE', #17180, #20365, #2957 ) ;
#19177 = ADVANCED_FACE ( 'NONE', ( #14869 ), #14764, .F. ) ;
#19178 = CYLINDRICAL_SURFACE ( 'NONE', #8915, 14.59999999999999964 ) ;
#19179 = VERTEX_POINT ( 'NONE', #14559 ) ;
#19180 = DIRECTION ( 'NONE',  ( 0.000000000000000000, 0.000000000000000000, -1.000000000000000000 ) ) ;
#19181 = DIRECTION ( 'NONE',  ( -0.000000000000000000, 1.000000000000000000, -0.000000000000000000 ) ) ;
#19182 = UNCERTAINTY_MEASURE_WITH_UNIT (LENGTH_MEASURE( 1.000000000000000082E-05 ), #20317, 'distance_accuracy_value', 'NONE');
#19183 = VERTEX_POINT ( 'NONE', #10133 ) ;
#19184 = LINE ( 'NONE', #119, #1138 ) ;
#19185 = CARTESIAN_POINT ( 'NONE',  ( -1.000000000000009104, 142.0976792249509231, 485.4122383872432351 ) ) ;
#19186 = COLOUR_RGB ( '', 0.66274510, 0.83137255, 0.94901961) ;
#19187 = EDGE_CURVE ( 'NONE', #19843, #296, #16288, .T. ) ;
#19188 = AXIS2_PLACEMENT_3D ( 'NONE', #1510, #15874, #3184 ) ;
#19189 = FACE_OUTER_BOUND ( 'NONE', #18887, .T. ) ;
#19190 = SURFACE_STYLE_USAGE ( .BOTH. , #12928 ) ;
#19191 = DIRECTION ( 'NONE',  ( 1.000000000000000000, 5.889072920838430686E-16, -0.000000000000000000 ) ) ;
#19192 = CARTESIAN_POINT ( 'NONE',  ( 25.99999999999996092, 0.000000000000000000, 31.00000000000004263 ) ) ;
#19193 = VERTEX_POINT ( 'NONE', #2183 ) ;
#19194 = PLANE ( 'NONE',  #2597 ) ;
#19195 = LINE ( 'NONE', #4989, #12189 ) ;
#19196 = CIRCLE ( 'NONE', #13306, 10.00000000000000888 ) ;
#19197 =( NAMED_UNIT ( * ) SI_UNIT ( $, .STERADIAN. ) SOLID_ANGLE_UNIT ( ) );
#19198 = ADVANCED_FACE ( 'NONE', ( #6952 ), #547, .F. ) ;
#19199 = VECTOR ( 'NONE', #4754, 1000.000000000000000 ) ;
#19200 = ORIENTED_EDGE ( 'NONE', *, *, #11630, .T. ) ;
#19201 = DIRECTION ( 'NONE',  ( -1.000000000000000000, -0.000000000000000000, -0.000000000000000000 ) ) ;
#19202 = EDGE_CURVE ( 'NONE', #345, #5312, #19682, .T. ) ;
#19203 = EDGE_LOOP ( 'NONE', ( #2955, #2367, #9846, #498 ) ) ;
#19204 = EDGE_LOOP ( 'NONE', ( #648, #9295, #16096 ) ) ;
#19205 = CIRCLE ( 'NONE', #5721, 15.25000000000000000 ) ;
#19206 = AXIS2_PLACEMENT_3D ( 'NONE', #8315, #6880, #13163 ) ;
#19207 = ORIENTED_EDGE ( 'NONE', *, *, #16601, .F. ) ;
#19208 = VERTEX_POINT ( 'NONE', #13531 ) ;
#19209 = DIRECTION ( 'NONE',  ( 0.000000000000000000, 0.000000000000000000, 1.000000000000000000 ) ) ;
#19210 = EDGE_CURVE ( 'NONE', #17253, #5436, #15389, .T. ) ;
#19211 = SURFACE_STYLE_FILL_AREA ( #11387 ) ;
#19212 = ORIENTED_EDGE ( 'NONE', *, *, #7241, .T. ) ;
#19213 = VECTOR ( 'NONE', #5847, 1000.000000000000227 ) ;
#19214 = CARTESIAN_POINT ( 'NONE',  ( -35.00000000000000000, 8.000000000000000000, -21.00000000000000000 ) ) ;
#19215 = AXIS2_PLACEMENT_3D ( 'NONE', #8190, #19486, #9829 ) ;
#19216 = DIRECTION ( 'NONE',  ( 1.000000000000000000, 5.889072920838430686E-16, -0.000000000000000000 ) ) ;
#19217 = ORIENTED_EDGE ( 'NONE', *, *, #20054, .F. ) ;
#19218 = LINE ( 'NONE', #16155, #8728 ) ;
#19219 = COLOUR_RGB ( '', 0.09019608, 0.27058824, 0.51372549) ;
#19220 = DIRECTION ( 'NONE',  ( -0.000000000000000000, -1.000000000000000000, 0.000000000000000000 ) ) ;
#19221 = SURFACE_SIDE_STYLE ('',( #1986 ) ) ;
#19222 = DIRECTION ( 'NONE',  ( 0.000000000000000000, 0.000000000000000000, 1.000000000000000000 ) ) ;
#19223 = EDGE_CURVE ( 'NONE', #6022, #183, #18261, .T. ) ;
#19224 = CARTESIAN_POINT ( 'NONE',  ( 423.8334540492694487, 191.8198460455371333, 168.2339398819845826 ) ) ;
#19225 = VECTOR ( 'NONE', #535, 1000.000000000000000 ) ;
#19226 = DIRECTION ( 'NONE',  ( 0.000000000000000000, 0.000000000000000000, 1.000000000000000000 ) ) ;
#19227 = AXIS2_PLACEMENT_3D ( 'NONE', #19955, #8939, #7307 ) ;
#19228 = EDGE_LOOP ( 'NONE', ( #15630, #19622, #1704, #19812, #10421 ) ) ;
#19229 = SURFACE_STYLE_USAGE ( .BOTH. , #8208 ) ;
#19230 = FILL_AREA_STYLE ('',( #2203 ) ) ;
#19231 = DIRECTION ( 'NONE',  ( 0.000000000000000000, 0.000000000000000000, -1.000000000000000000 ) ) ;
#19232 = DIRECTION ( 'NONE',  ( 0.000000000000000000, 0.000000000000000000, 1.000000000000000000 ) ) ;
#19233 = VECTOR ( 'NONE', #14473, 1000.000000000000000 ) ;
#19234 = EDGE_CURVE ( 'NONE', #6758, #16084, #4168, .T. ) ;
#19235 = EDGE_LOOP ( 'NONE', ( #8553, #9614, #1241, #13995, #8226, #14294 ) ) ;
#19236 = DIRECTION ( 'NONE',  ( -1.000000000000000000, -9.815121534730717399E-17, 0.000000000000000000 ) ) ;
#19237 = FACE_OUTER_BOUND ( 'NONE', #10183, .T. ) ;
#19238 = VECTOR ( 'NONE', #19109, 1000.000000000000000 ) ;
#19239 = ORIENTED_EDGE ( 'NONE', *, *, #14754, .F. ) ;
#19240 =( GEOMETRIC_REPRESENTATION_CONTEXT ( 3 ) GLOBAL_UNCERTAINTY_ASSIGNED_CONTEXT ( ( #4337 ) ) GLOBAL_UNIT_ASSIGNED_CONTEXT ( ( #19870, #2359, #7317 ) ) REPRESENTATION_CONTEXT ( 'NONE', 'WORKASPACE' ) );
#19241 = STYLED_ITEM ( 'NONE', ( #8256 ), #15094 ) ;
#19242 = VERTEX_POINT ( 'NONE', #8687 ) ;
#19243 = ORIENTED_EDGE ( 'NONE', *, *, #17597, .T. ) ;
#19244 = VECTOR ( 'NONE', #11301, 1000.000000000000000 ) ;
#19245 = ORIENTED_EDGE ( 'NONE', *, *, #12809, .F. ) ;
#19246 =( LENGTH_UNIT ( ) NAMED_UNIT ( * ) SI_UNIT ( .MILLI., .METRE. ) );
#19247 = CARTESIAN_POINT ( 'NONE',  ( 475.8334540492694487, 214.2156642432025251, 250.0000000000000000 ) ) ;
#19248 = AXIS2_PLACEMENT_3D ( 'NONE', #3636, #5286, #622 ) ;
#19249 = ORIENTED_EDGE ( 'NONE', *, *, #7129, .F. ) ;
#19250 = SURFACE_SIDE_STYLE ('',( #13092 ) ) ;
#19251 = CARTESIAN_POINT ( 'NONE',  ( 98.48937290013662960, 113.1299228374914350, 170.4174721992565082 ) ) ;
#19252 = EDGE_CURVE ( 'NONE', #5436, #16841, #18356, .T. ) ;
#19253 = ORIENTED_EDGE ( 'NONE', *, *, #17325, .F. ) ;
#19254 = VECTOR ( 'NONE', #2297, 1000.000000000000000 ) ;
#19255 = DIRECTION ( 'NONE',  ( 1.000000000000000000, 5.889072920838430686E-16, -0.000000000000000000 ) ) ;
#19256 = CARTESIAN_POINT ( 'NONE',  ( 30.99999999999999645, 3.000000000000000000, -25.99999999999999645 ) ) ;
#19257 = FILL_AREA_STYLE ('',( #14404 ) ) ;
#19258 = DIRECTION ( 'NONE',  ( -0.000000000000000000, 1.000000000000000000, -0.000000000000000000 ) ) ;
#19259 = CARTESIAN_POINT ( 'NONE',  ( 31.00000000000001421, 10.00000000000000000, 22.99999999999999645 ) ) ;
#19260 = EDGE_CURVE ( 'NONE', #17263, #19061, #4049, .T. ) ;
#19261 = CARTESIAN_POINT ( 'NONE',  ( 0.000000000000000000, 23.00000000000000000, -34.00000000000000000 ) ) ;
#19262 = CIRCLE ( 'NONE', #3804, 7.999999999999952038 ) ;
#19263 = DIRECTION ( 'NONE',  ( -0.000000000000000000, -0.000000000000000000, 1.000000000000000000 ) ) ;
#19264 = DIRECTION ( 'NONE',  ( -1.000000000000000000, -0.000000000000000000, -0.000000000000000000 ) ) ;
#19265 = CARTESIAN_POINT ( 'NONE',  ( 178.4893729001365728, 103.1299228374914776, 220.6387154965113382 ) ) ;
#19266 = VERTEX_POINT ( 'NONE', #2503 ) ;
#19267 = VECTOR ( 'NONE', #2960, 1000.000000000000000 ) ;
#19268 = ORIENTED_EDGE ( 'NONE', *, *, #12551, .T. ) ;
#19269 = AXIS2_PLACEMENT_3D ( 'NONE', #12336, #7697, #14179 ) ;
#19270 = VERTEX_POINT ( 'NONE', #15175 ) ;
#19271 = ORIENTED_EDGE ( 'NONE', *, *, #5353, .F. ) ;
#19272 = ORIENTED_EDGE ( 'NONE', *, *, #3781, .F. ) ;
#19273 = CARTESIAN_POINT ( 'NONE',  ( -31.00000000000005329, 10.00000000000000000, -26.00000000000000355 ) ) ;
#19274 = MECHANICAL_DESIGN_GEOMETRIC_PRESENTATION_REPRESENTATION (  '', ( #18274 ), #12360 ) ;
#19275 = CARTESIAN_POINT ( 'NONE',  ( -79.99999999999995737, 216.7545334744432921, 510.3921618609452935 ) ) ;
#19276 = FACE_BOUND ( 'NONE', #273, .T. ) ;
#19277 = CIRCLE ( 'NONE', #6443, 10.00000000000000888 ) ;
#19278 = LINE ( 'NONE', #397, #15916 ) ;
#19279 =( LENGTH_UNIT ( ) NAMED_UNIT ( * ) SI_UNIT ( .MILLI., .METRE. ) );
#19280 = CARTESIAN_POINT ( 'NONE',  ( 4.025000000000000355, 17.52499999999999858, 0.000000000000000000 ) ) ;
#19281 = EDGE_CURVE ( 'NONE', #16049, #12403, #18145, .T. ) ;
#19282 = DIRECTION ( 'NONE',  ( -0.000000000000000000, 1.000000000000000000, -0.000000000000000000 ) ) ;
#19283 = DIRECTION ( 'NONE',  ( -0.000000000000000000, -1.000000000000000000, -0.000000000000000000 ) ) ;
#19284 = AXIS2_PLACEMENT_3D ( 'NONE', #5798, #6204, #12385 ) ;
#19285 = ORIENTED_EDGE ( 'NONE', *, *, #17492, .T. ) ;
#19286 = SURFACE_STYLE_USAGE ( .BOTH. , #9909 ) ;
#19287 = ORIENTED_EDGE ( 'NONE', *, *, #9848, .F. ) ;
#19288 = DIRECTION ( 'NONE',  ( 0.000000000000000000, 0.000000000000000000, 1.000000000000000000 ) ) ;
#19289 = ORIENTED_EDGE ( 'NONE', *, *, #7753, .F. ) ;
#19290 = EDGE_CURVE ( 'NONE', #2774, #8147, #10633, .T. ) ;
#19291 = DIRECTION ( 'NONE',  ( -1.000000000000000000, 0.000000000000000000, 0.000000000000000000 ) ) ;
#19292 = DIRECTION ( 'NONE',  ( -0.000000000000000000, -0.000000000000000000, 1.000000000000000000 ) ) ;
#19293 = ORIENTED_EDGE ( 'NONE', *, *, #10398, .T. ) ;
#19294 = PLANE ( 'NONE',  #20247 ) ;
#19295 = DIRECTION ( 'NONE',  ( -1.000000000000000000, 0.000000000000000000, 0.000000000000000000 ) ) ;
#19296 = AXIS2_PLACEMENT_3D ( 'NONE', #601, #10188, #19449 ) ;
#19297 = FILL_AREA_STYLE_COLOUR ( '', #19170 ) ;
#19298 = CARTESIAN_POINT ( 'NONE',  ( -31.81980515339462912, 11.00000000000000000, 35.11980515339465825 ) ) ;
#19299 = ORIENTED_EDGE ( 'NONE', *, *, #19739, .F. ) ;
#19300 = DIRECTION ( 'NONE',  ( 0.000000000000000000, 0.000000000000000000, 1.000000000000000000 ) ) ;
#19301 = ADVANCED_FACE ( 'NONE', ( #4457, #7348, #18559, #19897, #927, #7250 ), #5903, .F. ) ;
#19302 = DIRECTION ( 'NONE',  ( 0.000000000000000000, 0.000000000000000000, 1.000000000000000000 ) ) ;
#19303 = VERTEX_POINT ( 'NONE', #4351 ) ;
#19304 = ADVANCED_FACE ( 'NONE', ( #1218 ), #2798, .T. ) ;
#19305 = ORIENTED_EDGE ( 'NONE', *, *, #5663, .T. ) ;
#19306 = VERTEX_POINT ( 'NONE', #4655 ) ;
#19307 = AXIS2_PLACEMENT_3D ( 'NONE', #3888, #5631, #6797 ) ;
#19308 = PLANE ( 'NONE',  #7463 ) ;
#19309 = VERTEX_POINT ( 'NONE', #217 ) ;
#19310 = DIRECTION ( 'NONE',  ( -6.120180426682197225E-17, 0.6235460666509320404, -0.7817866094812263578 ) ) ;
#19311 = CARTESIAN_POINT ( 'NONE',  ( 493.8117674897343363, 214.2156642432025251, 245.0000000000000000 ) ) ;
#19312 = VERTEX_POINT ( 'NONE', #12803 ) ;
#19313 = SURFACE_STYLE_USAGE ( .BOTH. , #17974 ) ;
#19314 = PLANE ( 'NONE',  #18173 ) ;
#19315 = EDGE_CURVE ( 'NONE', #7492, #8848, #13967, .T. ) ;
#19316 = CYLINDRICAL_SURFACE ( 'NONE', #14771, 8.999999999999952038 ) ;
#19317 = CARTESIAN_POINT ( 'NONE',  ( -31.00000000000003197, 68.00000000000000000, -22.99999999999999645 ) ) ;
#19318 = VERTEX_POINT ( 'NONE', #3112 ) ;
#19319 = FACE_BOUND ( 'NONE', #2822, .T. ) ;
#19320 = SURFACE_SIDE_STYLE ('',( #17778 ) ) ;
#19321 = DIRECTION ( 'NONE',  ( -0.000000000000000000, -1.000000000000000000, -0.000000000000000000 ) ) ;
#19322 = ADVANCED_FACE ( 'NONE', ( #6313 ), #9582, .F. ) ;
#19323 = FACE_OUTER_BOUND ( 'NONE', #16099, .T. ) ;
#19324 = EDGE_LOOP ( 'NONE', ( #16789, #16154, #19878, #1187, #344 ) ) ;
#19325 = EDGE_CURVE ( 'NONE', #296, #11484, #18857, .T. ) ;
#19326 = EDGE_LOOP ( 'NONE', ( #12545, #7169 ) ) ;
#19327 = ADVANCED_FACE ( 'NONE', ( #11051 ), #16305, .F. ) ;
#19328 = AXIS2_PLACEMENT_3D ( 'NONE', #10000, #14837, #7128 ) ;
#19329 = ORIENTED_EDGE ( 'NONE', *, *, #14734, .F. ) ;
#19330 = PRESENTATION_STYLE_ASSIGNMENT (( #8125 ) ) ;
#19331 = APPLICATION_CONTEXT ( 'automotive_design' ) ;
#19332 = CARTESIAN_POINT ( 'NONE',  ( 25.99999999999999645, 0.000000000000000000, 40.00000000000002132 ) ) ;
#19333 = EDGE_LOOP ( 'NONE', ( #13242, #1107 ) ) ;
#19334 = CARTESIAN_POINT ( 'NONE',  ( -34.99999999999996447, 0.000000000000000000, 40.00000000000000711 ) ) ;
#19335 =( NAMED_UNIT ( * ) PLANE_ANGLE_UNIT ( ) SI_UNIT ( $, .RADIAN. ) );
#19336 = EDGE_CURVE ( 'NONE', #12894, #6958, #10682, .T. ) ;
#19337 = ORIENTED_EDGE ( 'NONE', *, *, #2305, .T. ) ;
#19338 = CARTESIAN_POINT ( 'NONE',  ( -79.99999999999995737, 216.7545334744432921, 512.1946179577817020 ) ) ;
#19339 = CARTESIAN_POINT ( 'NONE',  ( -0.000000000000000000, 167.9162550801369491, 250.0000000000000000 ) ) ;
#19340 = CARTESIAN_POINT ( 'NONE',  ( 0.1987446979796453350, 139.8600507635789825, 489.1673953262136934 ) ) ;
#19341 = DIRECTION ( 'NONE',  ( 0.000000000000000000, 0.000000000000000000, 1.000000000000000000 ) ) ;
#19342 = LINE ( 'NONE', #9975, #9144 ) ;
#19343 = CARTESIAN_POINT ( 'NONE',  ( -77.99033078109006567, 49.66333933884486385, 252.0000000000000000 ) ) ;
#19344 = DIRECTION ( 'NONE',  ( 0.000000000000000000, 1.000000000000000000, 0.000000000000000000 ) ) ;
#19345 = AXIS2_PLACEMENT_3D ( 'NONE', #15334, #10784, #20033 ) ;
#19346 = DIRECTION ( 'NONE',  ( 1.000000000000000000, 1.047380211910525299E-15, -0.000000000000000000 ) ) ;
#19347 = ORIENTED_EDGE ( 'NONE', *, *, #6018, .F. ) ;
#19348 = ORIENTED_EDGE ( 'NONE', *, *, #18132, .T. ) ;
#19349 = ORIENTED_EDGE ( 'NONE', *, *, #14530, .F. ) ;
#19350 = ORIENTED_EDGE ( 'NONE', *, *, #8849, .F. ) ;
#19351 = EDGE_CURVE ( 'NONE', #6321, #13610, #15901, .T. ) ;
#19352 = CARTESIAN_POINT ( 'NONE',  ( 423.8334540492694487, 191.8198460455371333, 178.2339398819846110 ) ) ;
#19353 = DIRECTION ( 'NONE',  ( -0.000000000000000000, -0.000000000000000000, 1.000000000000000000 ) ) ;
#19355 = EDGE_CURVE ( 'NONE', #10076, #19819, #1631, .T. ) ;
#19354 = PRESENTATION_LAYER_ASSIGNMENT (  '', '', ( #7848 ) ) ;
#19356 = LINE ( 'NONE', #1931, #1749 ) ;
#19357 = EDGE_CURVE ( 'NONE', #11769, #16198, #1782, .T. ) ;
#19358 = DIRECTION ( 'NONE',  ( 1.000000000000000000, 0.000000000000000000, 0.000000000000000000 ) ) ;
#19359 = DIRECTION ( 'NONE',  ( 0.000000000000000000, 0.000000000000000000, -1.000000000000000000 ) ) ;
#19360 = CARTESIAN_POINT ( 'NONE',  ( 153.4893729001366580, 145.9162550801369491, -140.0000000000001137 ) ) ;
#19361 = FACE_OUTER_BOUND ( 'NONE', #4365, .T. ) ;
#19362 = FILL_AREA_STYLE_COLOUR ( '', #6077 ) ;
#19363 = DIRECTION ( 'NONE',  ( 1.000000000000000000, 0.000000000000000000, 0.000000000000000000 ) ) ;
#19364 = PLANE ( 'NONE',  #14908 ) ;
#19365 = CARTESIAN_POINT ( 'NONE',  ( 153.4893729001366864, 113.1299228374914634, 170.4174721992565082 ) ) ;
#19366 = CARTESIAN_POINT ( 'NONE',  ( 26.00000000000001066, 0.000000000000000000, -31.00000000000002487 ) ) ;
#19367 = CIRCLE ( 'NONE', #18044, 0.9999999999999995559 ) ;
#19368 = VERTEX_POINT ( 'NONE', #14230 ) ;
#19369 = CARTESIAN_POINT ( 'NONE',  ( 3.000000000000000000, 6.000000000000000000, 22.00000000000000000 ) ) ;
#19370 = UNCERTAINTY_MEASURE_WITH_UNIT (LENGTH_MEASURE( 1.000000000000000082E-05 ), #1095, 'distance_accuracy_value', 'NONE');
#19371 = EDGE_LOOP ( 'NONE', ( #14496, #16226, #7736, #14472, #19662 ) ) ;
#19372 = ORIENTED_EDGE ( 'NONE', *, *, #4428, .T. ) ;
#19373 = EDGE_CURVE ( 'NONE', #1752, #20152, #20308, .T. ) ;
#19374 = DIRECTION ( 'NONE',  ( 0.000000000000000000, 0.000000000000000000, 1.000000000000000000 ) ) ;
#19375 = ORIENTED_EDGE ( 'NONE', *, *, #1036, .T. ) ;
#19376 = UNCERTAINTY_MEASURE_WITH_UNIT (LENGTH_MEASURE( 1.000000000000000082E-05 ), #19048, 'distance_accuracy_value', 'NONE');
#19377 = FACE_OUTER_BOUND ( 'NONE', #551, .T. ) ;
#19378 = PLANE ( 'NONE',  #11873 ) ;
#19379 = VERTEX_POINT ( 'NONE', #4556 ) ;
#19380 = CARTESIAN_POINT ( 'NONE',  ( -20.99999999999999645, 8.000000000000000000, -31.00000000000003908 ) ) ;
#19381 = MECHANICAL_DESIGN_GEOMETRIC_PRESENTATION_REPRESENTATION (  '', ( #15132 ), #12158 ) ;
#19382 = DIRECTION ( 'NONE',  ( 0.000000000000000000, 0.000000000000000000, -1.000000000000000000 ) ) ;
#19383 = CIRCLE ( 'NONE', #17401, 2.999999999999995559 ) ;
#19384 = VECTOR ( 'NONE', #7586, 1000.000000000000000 ) ;
#19385 = CARTESIAN_POINT ( 'NONE',  ( -79.99999999999995737, 140.1563709946295262, 488.5655098179835818 ) ) ;
#19386 = CYLINDRICAL_SURFACE ( 'NONE', #18504, 1.999999999999997113 ) ;
#19387 = DIRECTION ( 'NONE',  ( -0.000000000000000000, -1.000000000000000000, -0.000000000000000000 ) ) ;
#19388 = CARTESIAN_POINT ( 'NONE',  ( 463.8334540492693350, 191.8198460455371333, 14.99421986894475012 ) ) ;
#19389 = VERTEX_POINT ( 'NONE', #11140 ) ;
#19390 = CYLINDRICAL_SURFACE ( 'NONE', #13148, 2.500000000000002220 ) ;
#19391 = FILL_AREA_STYLE_COLOUR ( '', #454 ) ;
#19392 = FACE_OUTER_BOUND ( 'NONE', #8729, .T. ) ;
#19393 = DIRECTION ( 'NONE',  ( 0.000000000000000000, 0.000000000000000000, -1.000000000000000000 ) ) ;
#19394 = ORIENTED_EDGE ( 'NONE', *, *, #14289, .F. ) ;
#19395 = MECHANICAL_DESIGN_GEOMETRIC_PRESENTATION_REPRESENTATION (  '', ( #17105 ), #1952 ) ;
#19396 = ORIENTED_EDGE ( 'NONE', *, *, #8997, .F. ) ;
#19397 = ORIENTED_EDGE ( 'NONE', *, *, #6833, .T. ) ;
#19398 = CARTESIAN_POINT ( 'NONE',  ( -1.224646799147350495E-16, 41.00000000000000711, 6.000000000000000000 ) ) ;
#19399 = VERTEX_POINT ( 'NONE', #7645 ) ;
#19400 = UNCERTAINTY_MEASURE_WITH_UNIT (LENGTH_MEASURE( 1.000000000000000082E-05 ), #10454, 'distance_accuracy_value', 'NONE');
#19401 = DIRECTION ( 'NONE',  ( 1.000000000000000000, 2.135044278125300850E-16, -0.000000000000000000 ) ) ;
#19402 = DIRECTION ( 'NONE',  ( -0.000000000000000000, 1.000000000000000000, -0.000000000000000000 ) ) ;
#19403 = ORIENTED_EDGE ( 'NONE', *, *, #3831, .T. ) ;
#19404 = CARTESIAN_POINT ( 'NONE',  ( 463.8334540492693350, 214.2156642432025251, 250.0000000000000000 ) ) ;
#19405 =( LENGTH_UNIT ( ) NAMED_UNIT ( * ) SI_UNIT ( .MILLI., .METRE. ) );
#19406 = DIRECTION ( 'NONE',  ( -1.000000000000000000, 0.000000000000000000, 0.000000000000000000 ) ) ;
#19407 = AXIS2_PLACEMENT_3D ( 'NONE', #12746, #14167, #5008 ) ;
#19408 = PRESENTATION_STYLE_ASSIGNMENT (( #2405 ) ) ;
#19409 = CARTESIAN_POINT ( 'NONE',  ( 21.00000000000000000, 19.00000000000000000, 31.00000000000006395 ) ) ;
#19410 = VERTEX_POINT ( 'NONE', #13930 ) ;
#19411 = SURFACE_STYLE_FILL_AREA ( #8421 ) ;
#19412 = CARTESIAN_POINT ( 'NONE',  ( 30.99999999999997868, 10.00000000000000000, -30.99999999999999645 ) ) ;
#19413 = CARTESIAN_POINT ( 'NONE',  ( -31.81980515339462912, 11.00000000000000000, 28.51980515339464617 ) ) ;
#19414 = FILL_AREA_STYLE_COLOUR ( '', #11970 ) ;
#19415 = CARTESIAN_POINT ( 'NONE',  ( -19.00000000000001776, 10.00000000000000000, 36.00000000000000711 ) ) ;
#19416 = ADVANCED_FACE ( 'NONE', ( #6116 ), #10839, .F. ) ;
#19417 = ORIENTED_EDGE ( 'NONE', *, *, #17967, .F. ) ;
#19418 = ORIENTED_EDGE ( 'NONE', *, *, #16118, .F. ) ;
#19419 = AXIS2_PLACEMENT_3D ( 'NONE', #5880, #1100, #2968 ) ;
#19420 = AXIS2_PLACEMENT_3D ( 'NONE', #2795, #4347, #7050 ) ;
#19421 = VERTEX_POINT ( 'NONE', #9287 ) ;
#19422 = DIRECTION ( 'NONE',  ( -0.000000000000000000, -1.000000000000000000, -0.000000000000000000 ) ) ;
#19423 = CARTESIAN_POINT ( 'NONE',  ( 21.00000000000000000, 8.000000000000000000, -31.00000000000003908 ) ) ;
#19424 = ORIENTED_EDGE ( 'NONE', *, *, #4611, .F. ) ;
#19425 = EDGE_CURVE ( 'NONE', #16895, #6137, #15602, .T. ) ;
#19426 = SURFACE_STYLE_FILL_AREA ( #13181 ) ;
#19427 = ORIENTED_EDGE ( 'NONE', *, *, #19351, .F. ) ;
#19428 = CARTESIAN_POINT ( 'NONE',  ( -23.00000000000002487, 10.00000000000000000, -31.00000000000003553 ) ) ;
#19429 = DIRECTION ( 'NONE',  ( 1.000000000000000000, 0.000000000000000000, -0.000000000000000000 ) ) ;
#19430 = SURFACE_SIDE_STYLE ('',( #13184 ) ) ;
#19431 = DIRECTION ( 'NONE',  ( 1.000000000000000000, 0.000000000000000000, 0.000000000000000000 ) ) ;
#19432 = EDGE_CURVE ( 'NONE', #2723, #14489, #3420, .T. ) ;
#19433 = FACE_OUTER_BOUND ( 'NONE', #4947, .T. ) ;
#19434 = VECTOR ( 'NONE', #8287, 1000.000000000000000 ) ;
#19435 = EDGE_CURVE ( 'NONE', #951, #5981, #11452, .T. ) ;
#19436 = AXIS2_PLACEMENT_3D ( 'NONE', #17738, #8672, #16518 ) ;
#19437 = DIRECTION ( 'NONE',  ( 1.000000000000000000, 1.197852309262419498E-15, -0.000000000000000000 ) ) ;
#19438 = DIRECTION ( 'NONE',  ( 1.000000000000000000, 0.000000000000000000, 1.156482317317870344E-15 ) ) ;
#19439 = ORIENTED_EDGE ( 'NONE', *, *, #1395, .T. ) ;
#19440 = DIRECTION ( 'NONE',  ( 1.000000000000000000, -0.000000000000000000, -0.000000000000000000 ) ) ;
#19441 = LINE ( 'NONE', #5347, #6250 ) ;
#19442 = EDGE_LOOP ( 'NONE', ( #19638, #19821, #3018, #7032 ) ) ;
#19443 = EDGE_CURVE ( 'NONE', #19903, #8271, #13123, .T. ) ;
#19444 = EDGE_CURVE ( 'NONE', #19815, #14619, #8260, .T. ) ;
#19445 = VERTEX_POINT ( 'NONE', #313 ) ;
#19446 = ORIENTED_EDGE ( 'NONE', *, *, #8799, .F. ) ;
#19447 = ORIENTED_EDGE ( 'NONE', *, *, #1635, .T. ) ;
#19448 = VERTEX_POINT ( 'NONE', #13215 ) ;
#19449 = DIRECTION ( 'NONE',  ( 0.000000000000000000, 1.000000000000000000, 0.000000000000000000 ) ) ;
#19450 =( LENGTH_UNIT ( ) NAMED_UNIT ( * ) SI_UNIT ( .MILLI., .METRE. ) );
#19451 = CARTESIAN_POINT ( 'NONE',  ( 0.9999999999999876765, 138.7545334744432637, 501.8237260975781737 ) ) ;
#19452 = EDGE_CURVE ( 'NONE', #3836, #4888, #16321, .T. ) ;
#19453 = SPHERICAL_SURFACE ( 'NONE', #6254, 1.000000000000000000 ) ;
#19454 = DIRECTION ( 'NONE',  ( -0.000000000000000000, -1.000000000000000000, -0.000000000000000000 ) ) ;
#19455 = FACE_BOUND ( 'NONE', #15037, .T. ) ;
#19456 = DIRECTION ( 'NONE',  ( 0.000000000000000000, 0.000000000000000000, 1.000000000000000000 ) ) ;
#19457 = DIRECTION ( 'NONE',  ( 0.000000000000000000, -1.000000000000000000, 0.000000000000000000 ) ) ;
#19458 = CARTESIAN_POINT ( 'NONE',  ( -1.776356839400249676E-15, 0.000000000000000000, 0.000000000000000000 ) ) ;
#19459 = EDGE_CURVE ( 'NONE', #17220, #16810, #9701, .T. ) ;
#19460 = FILL_AREA_STYLE ('',( #6931 ) ) ;
#19461 = VECTOR ( 'NONE', #19733, 1000.000000000000000 ) ;
#19462 = ORIENTED_EDGE ( 'NONE', *, *, #17179, .F. ) ;
#19463 = COLOUR_RGB ( '', 0.31764706, 0.68627451, 0.89019608) ;
#19464 = CARTESIAN_POINT ( 'NONE',  ( 1.050000000000000044, 16.38749999999999929, 0.000000000000000000 ) ) ;
#19465 = ORIENTED_EDGE ( 'NONE', *, *, #11142, .F. ) ;
#19466 = EDGE_LOOP ( 'NONE', ( #1470, #15627, #5302, #14228, #17768, #7467 ) ) ;
#19467 = ORIENTED_EDGE ( 'NONE', *, *, #8091, .F. ) ;
#19468 = SURFACE_STYLE_USAGE ( .BOTH. , #18034 ) ;
#19469 = STYLED_ITEM ( 'NONE', ( #7402 ), #13518 ) ;
#19470 = MECHANICAL_DESIGN_GEOMETRIC_PRESENTATION_REPRESENTATION (  '', ( #7974 ), #9590 ) ;
#19471 = DIRECTION ( 'NONE',  ( 0.000000000000000000, 0.000000000000000000, -1.000000000000000000 ) ) ;
#19472 = ORIENTED_EDGE ( 'NONE', *, *, #5322, .F. ) ;
#19473 = DIRECTION ( 'NONE',  ( 0.000000000000000000, 0.000000000000000000, -1.000000000000000000 ) ) ;
#19474 = CARTESIAN_POINT ( 'NONE',  ( -23.00000000000003197, 0.000000000000000000, 34.00000000000000711 ) ) ;
#19475 = LINE ( 'NONE', #16230, #3050 ) ;
#19476 = EDGE_CURVE ( 'NONE', #19183, #298, #5181, .T. ) ;
#19477 = LINE ( 'NONE', #2266, #7436 ) ;
#19478 = LINE ( 'NONE', #6851, #17518 ) ;
#19479 = DIRECTION ( 'NONE',  ( 1.000000000000000000, -0.000000000000000000, -0.000000000000000000 ) ) ;
#19480 = DIRECTION ( 'NONE',  ( -0.000000000000000000, -1.000000000000000000, -0.000000000000000000 ) ) ;
#19481 = VECTOR ( 'NONE', #4760, 1000.000000000000000 ) ;
#19482 = VERTEX_POINT ( 'NONE', #13317 ) ;
#19483 = DIRECTION ( 'NONE',  ( 6.123031769111888756E-17, 0.000000000000000000, 1.000000000000000000 ) ) ;
#19484 = PRESENTATION_LAYER_ASSIGNMENT (  '', '', ( #7982 ) ) ;
#19485 =( NAMED_UNIT ( * ) PLANE_ANGLE_UNIT ( ) SI_UNIT ( $, .RADIAN. ) );
#19486 = DIRECTION ( 'NONE',  ( -0.000000000000000000, -1.000000000000000000, -0.000000000000000000 ) ) ;
#19487 = VECTOR ( 'NONE', #10890, 1000.000000000000114 ) ;
#19488 = VECTOR ( 'NONE', #10386, 1000.000000000000000 ) ;
#19489 = VERTEX_POINT ( 'NONE', #19169 ) ;
#19490 = ORIENTED_EDGE ( 'NONE', *, *, #5977, .F. ) ;
#19491 = CARTESIAN_POINT ( 'NONE',  ( -31.81980515339462912, 0.000000000000000000, -31.81980515339465043 ) ) ;
#19492 = VECTOR ( 'NONE', #13071, 1000.000000000000000 ) ;
#19493 = ORIENTED_EDGE ( 'NONE', *, *, #9139, .T. ) ;
#19494 = LINE ( 'NONE', #2284, #12307 ) ;
#19495 = LINE ( 'NONE', #5411, #18409 ) ;
#19496 = ORIENTED_EDGE ( 'NONE', *, *, #19850, .F. ) ;
#19497 = DIRECTION ( 'NONE',  ( 0.000000000000000000, 0.000000000000000000, -1.000000000000000000 ) ) ;
#19498 = CARTESIAN_POINT ( 'NONE',  ( 25.99999999999996092, 3.000000000000000000, -31.00000000000003197 ) ) ;
#19499 = VECTOR ( 'NONE', #4248, 1000.000000000000000 ) ;
#19500 = AXIS2_PLACEMENT_3D ( 'NONE', #12908, #17825, #5179 ) ;
#19501 = FACE_OUTER_BOUND ( 'NONE', #6031, .T. ) ;
#19502 = EDGE_LOOP ( 'NONE', ( #11171, #15551, #10845, #10738, #4637 ) ) ;
#19503 = CARTESIAN_POINT ( 'NONE',  ( -31.00000000000000000, 19.00000000000000000, -31.00000000000000000 ) ) ;
#19504 = CYLINDRICAL_SURFACE ( 'NONE', #19159, 7.999999999999996447 ) ;
#19505 =( LENGTH_UNIT ( ) NAMED_UNIT ( * ) SI_UNIT ( .MILLI., .METRE. ) );
#19506 = DIRECTION ( 'NONE',  ( -0.000000000000000000, 0.000000000000000000, 1.000000000000000000 ) ) ;
#19507 = DIRECTION ( 'NONE',  ( -3.657132581846951845E-29, 1.000000000000000000, -3.491481338843133355E-15 ) ) ;
#19508 = EDGE_CURVE ( 'NONE', #8713, #11104, #6621, .T. ) ;
#19509 = EDGE_LOOP ( 'NONE', ( #5736, #8509 ) ) ;
#19510 = VECTOR ( 'NONE', #6924, 1000.000000000000000 ) ;
#19511 = ORIENTED_EDGE ( 'NONE', *, *, #14451, .F. ) ;
#19512 = VERTEX_POINT ( 'NONE', #19366 ) ;
#19513 = VECTOR ( 'NONE', #8334, 1000.000000000000000 ) ;
#19514 = VECTOR ( 'NONE', #3041, 1000.000000000000000 ) ;
#19515 = ORIENTED_EDGE ( 'NONE', *, *, #1070, .F. ) ;
#19516 = VERTEX_POINT ( 'NONE', #7029 ) ;
#19517 = CYLINDRICAL_SURFACE ( 'NONE', #18142, 2.500000000000002220 ) ;
#19518 = CARTESIAN_POINT ( 'NONE',  ( 22.99999999999997513, 10.00000000000000000, 31.00000000000005684 ) ) ;
#19519 = VERTEX_POINT ( 'NONE', #17828 ) ;
#19520 = DIRECTION ( 'NONE',  ( 0.000000000000000000, 1.000000000000000000, 0.000000000000000000 ) ) ;
#19521 = AXIS2_PLACEMENT_3D ( 'NONE', #7359, #1031, #13645 ) ;
#19522 = LINE ( 'NONE', #6987, #15558 ) ;
#19523 = MECHANICAL_DESIGN_GEOMETRIC_PRESENTATION_REPRESENTATION (  '', ( #1407 ), #13315 ) ;
#19524 = ADVANCED_FACE ( 'NONE', ( #14437 ), #3626, .T. ) ;
#19525 = CARTESIAN_POINT ( 'NONE',  ( 21.00000000000000000, 19.00000000000000000, -35.00000000000000711 ) ) ;
#19526 = COLOUR_RGB ( '', 0.09019608, 0.27058824, 0.51372549) ;
#19527 = DIRECTION ( 'NONE',  ( 0.000000000000000000, 1.000000000000000000, 0.000000000000000000 ) ) ;
#19528 = LINE ( 'NONE', #13097, #9707 ) ;
#19529 =( LENGTH_UNIT ( ) NAMED_UNIT ( * ) SI_UNIT ( .MILLI., .METRE. ) );
#19530 = DIRECTION ( 'NONE',  ( 0.000000000000000000, 1.000000000000000000, 0.000000000000000000 ) ) ;
#19531 = STYLED_ITEM ( 'NONE', ( #2272 ), #19198 ) ;
#19532 = MECHANICAL_DESIGN_GEOMETRIC_PRESENTATION_REPRESENTATION (  '', ( #19241 ), #5752 ) ;
#19533 = FACE_BOUND ( 'NONE', #18717, .T. ) ;
#19534 = VECTOR ( 'NONE', #10223, 1000.000000000000000 ) ;
#19535 = LINE ( 'NONE', #6999, #1926 ) ;
#19536 = CARTESIAN_POINT ( 'NONE',  ( 0.000000000000000000, 66.00000000000000000, -5.741599279633704455E-16 ) ) ;
#19537 = EDGE_LOOP ( 'NONE', ( #13964, #18889, #7643, #14239 ) ) ;
#19538 =( GEOMETRIC_REPRESENTATION_CONTEXT ( 3 ) GLOBAL_UNCERTAINTY_ASSIGNED_CONTEXT ( ( #7065 ) ) GLOBAL_UNIT_ASSIGNED_CONTEXT ( ( #17402, #6601, #14326 ) ) REPRESENTATION_CONTEXT ( 'NONE', 'WORKASPACE' ) );
#19539 = EDGE_CURVE ( 'NONE', #11502, #4146, #11347, .T. ) ;
#19540 = VECTOR ( 'NONE', #16603, 1000.000000000000000 ) ;
#19541 = UNCERTAINTY_MEASURE_WITH_UNIT (LENGTH_MEASURE( 1.000000000000000082E-05 ), #5342, 'distance_accuracy_value', 'NONE');
#19542 = VECTOR ( 'NONE', #7555, 1000.000000000000000 ) ;
#19543 = ORIENTED_EDGE ( 'NONE', *, *, #15906, .F. ) ;
#19544 = EDGE_CURVE ( 'NONE', #1665, #11661, #14842, .T. ) ;
#19545 = ORIENTED_EDGE ( 'NONE', *, *, #2045, .F. ) ;
#19546 = ORIENTED_EDGE ( 'NONE', *, *, #15550, .F. ) ;
#19547 =( GEOMETRIC_REPRESENTATION_CONTEXT ( 3 ) GLOBAL_UNCERTAINTY_ASSIGNED_CONTEXT ( ( #5385 ) ) GLOBAL_UNIT_ASSIGNED_CONTEXT ( ( #10755, #6328, #15725 ) ) REPRESENTATION_CONTEXT ( 'NONE', 'WORKASPACE' ) );
#19548 = VECTOR ( 'NONE', #16414, 1000.000000000000000 ) ;
#19549 = CARTESIAN_POINT ( 'NONE',  ( 26.00000000000000355, 19.00000000000000000, -31.00000000000004263 ) ) ;
#19550 = AXIS2_PLACEMENT_3D ( 'NONE', #5177, #17822, #11448 ) ;
#19551 = CARTESIAN_POINT ( 'NONE',  ( -211.5106270998635409, 113.1299228374912502, 170.4174721992565082 ) ) ;
#19552 = CARTESIAN_POINT ( 'NONE',  ( -34.99999999999999289, 0.000000000000000000, -35.00000000000000711 ) ) ;
#19553 = VECTOR ( 'NONE', #6312, 1000.000000000000000 ) ;
#19554 = LINE ( 'NONE', #5466, #11645 ) ;
#19555 = LINE ( 'NONE', #16710, #2596 ) ;
#19556 = EDGE_CURVE ( 'NONE', #11244, #1495, #1435, .T. ) ;
#19557 =( LENGTH_UNIT ( ) NAMED_UNIT ( * ) SI_UNIT ( .MILLI., .METRE. ) );
#19558 = STYLED_ITEM ( 'NONE', ( #14946 ), #2057 ) ;
#19559 = SURFACE_STYLE_USAGE ( .BOTH. , #13310 ) ;
#19560 = LINE ( 'NONE', #810, #11032 ) ;
#19561 = AXIS2_PLACEMENT_3D ( 'NONE', #7290, #12320, #10469 ) ;
#19562 = DIRECTION ( 'NONE',  ( 0.000000000000000000, 1.000000000000000000, 0.000000000000000000 ) ) ;
#19563 = EDGE_CURVE ( 'NONE', #17153, #5319, #14744, .T. ) ;
#19564 = CARTESIAN_POINT ( 'NONE',  ( -79.96195573192551365, 139.0956700764377558, 488.6001242439256202 ) ) ;
#19565 = CARTESIAN_POINT ( 'NONE',  ( -30.99999999999999645, 68.00000000000000000, -30.99999999999999289 ) ) ;
#19566 = FACE_OUTER_BOUND ( 'NONE', #4939, .T. ) ;
#19567 = AXIS2_PLACEMENT_3D ( 'NONE', #14864, #1015, #15075 ) ;
#19568 = DIRECTION ( 'NONE',  ( 1.000000000000000000, 0.000000000000000000, 0.000000000000000000 ) ) ;
#19569 = AXIS2_PLACEMENT_3D ( 'NONE', #2903, #1454, #4877 ) ;
#19570 = MECHANICAL_DESIGN_GEOMETRIC_PRESENTATION_REPRESENTATION (  '', ( #2477 ), #7103 ) ;
#19571 = EDGE_CURVE ( 'NONE', #17808, #7735, #11674, .T. ) ;
#19572 = VERTEX_POINT ( 'NONE', #9906 ) ;
#19573 = ORIENTED_EDGE ( 'NONE', *, *, #17957, .T. ) ;
#19574 = PRESENTATION_LAYER_ASSIGNMENT (  '', '', ( #18274 ) ) ;
#19575 = DIRECTION ( 'NONE',  ( 1.000000000000000000, -0.000000000000000000, -1.450371633464475582E-15 ) ) ;
#19576 = UNCERTAINTY_MEASURE_WITH_UNIT (LENGTH_MEASURE( 1.000000000000000082E-05 ), #3802, 'distance_accuracy_value', 'NONE');
#19577 = VERTEX_POINT ( 'NONE', #13020 ) ;
#19578 = CIRCLE ( 'NONE', #15678, 2.500000000000002220 ) ;
#19579 = EDGE_CURVE ( 'NONE', #4262, #3611, #16214, .T. ) ;
#19580 = CARTESIAN_POINT ( 'NONE',  ( 498.8334540492693918, 191.8198460455371333, 14.99421986894475012 ) ) ;
#19581 = UNCERTAINTY_MEASURE_WITH_UNIT (LENGTH_MEASURE( 1.000000000000000082E-05 ), #4229, 'distance_accuracy_value', 'NONE');
#19582 = ORIENTED_EDGE ( 'NONE', *, *, #14565, .T. ) ;
#19583 = ADVANCED_FACE ( 'NONE', ( #611 ), #3829, .F. ) ;
#19584 = LINE ( 'NONE', #5491, #1772 ) ;
#19585 = CARTESIAN_POINT ( 'NONE',  ( 26.00000000000000000, 19.00000000000000000, 31.00000000000003197 ) ) ;
#19586 = DIRECTION ( 'NONE',  ( 0.000000000000000000, 1.000000000000000000, 0.000000000000000000 ) ) ;
#19587 = DIRECTION ( 'NONE',  ( 1.000000000000000000, 5.889072920838430686E-16, -0.000000000000000000 ) ) ;
#19588 = CARTESIAN_POINT ( 'NONE',  ( -80.33275375302500265, 138.8974262895977745, 489.3169310699432231 ) ) ;
#19589 = DIRECTION ( 'NONE',  ( 0.000000000000000000, 1.000000000000000000, 0.000000000000000000 ) ) ;
#19590 = VERTEX_POINT ( 'NONE', #5566 ) ;
#19591 = CARTESIAN_POINT ( 'NONE',  ( -80.99999999999995737, 140.4048636633015406, 500.8237260975782874 ) ) ;
#19592 = CARTESIAN_POINT ( 'NONE',  ( 30.99999999999997513, 10.00000000000000000, 30.99999999999999645 ) ) ;
#19593 = AXIS2_PLACEMENT_3D ( 'NONE', #448, #8868, #6863 ) ;
#19594 = ORIENTED_EDGE ( 'NONE', *, *, #6217, .T. ) ;
#19595 = EDGE_CURVE ( 'NONE', #12469, #11049, #4142, .T. ) ;
#19596 = ORIENTED_EDGE ( 'NONE', *, *, #9808, .T. ) ;
#19597 = ORIENTED_EDGE ( 'NONE', *, *, #6258, .T. ) ;
#19598 = VECTOR ( 'NONE', #15561, 1000.000000000000000 ) ;
#19599 = EDGE_LOOP ( 'NONE', ( #13067, #341, #4464, #7014 ) ) ;
#19600 = EDGE_CURVE ( 'NONE', #3926, #5312, #7083, .T. ) ;
#19601 = FACE_OUTER_BOUND ( 'NONE', #11350, .T. ) ;
#19602 = UNCERTAINTY_MEASURE_WITH_UNIT (LENGTH_MEASURE( 1.000000000000000082E-05 ), #5486, 'distance_accuracy_value', 'NONE');
#19603 = CIRCLE ( 'NONE', #10098, 10.00000000000000888 ) ;
#19604 = ORIENTED_EDGE ( 'NONE', *, *, #19678, .T. ) ;
#19605 = CARTESIAN_POINT ( 'NONE',  ( -79.99999999999995737, 316.7545334744432353, 515.1946179577817020 ) ) ;
#19606 = DIRECTION ( 'NONE',  ( 0.000000000000000000, 0.000000000000000000, -1.000000000000000000 ) ) ;
#19607 = DIRECTION ( 'NONE',  ( 7.715811803773179210E-14, 0.000000000000000000, 1.000000000000000000 ) ) ;
#19608 = ADVANCED_FACE ( 'NONE', ( #16619 ), #8774, .F. ) ;
#19609 = FILL_AREA_STYLE_COLOUR ( '', #17279 ) ;
#19610 = DIRECTION ( 'NONE',  ( -0.000000000000000000, -0.000000000000000000, 1.000000000000000000 ) ) ;
#19611 = CARTESIAN_POINT ( 'NONE',  ( 53.48937290013659407, 127.7247684487574588, 254.0000000000000000 ) ) ;
#19612 = VERTEX_POINT ( 'NONE', #16720 ) ;
#19613 = CARTESIAN_POINT ( 'NONE',  ( 153.4893729001366864, 113.1299228374914634, 79.58252780074349175 ) ) ;
#19614 = DIRECTION ( 'NONE',  ( 0.000000000000000000, 0.000000000000000000, -1.000000000000000000 ) ) ;
#19615 = SURFACE_STYLE_USAGE ( .BOTH. , #13376 ) ;
#19616 = PLANE ( 'NONE',  #16535 ) ;
#19617 = ORIENTED_EDGE ( 'NONE', *, *, #14654, .F. ) ;
#19618 = VECTOR ( 'NONE', #13269, 1000.000000000000000 ) ;
#19619 = ORIENTED_EDGE ( 'NONE', *, *, #18242, .F. ) ;
#19620 = ORIENTED_EDGE ( 'NONE', *, *, #6604, .T. ) ;
#19621 = EDGE_LOOP ( 'NONE', ( #4962, #7527, #19127, #10462 ) ) ;
#19622 = ORIENTED_EDGE ( 'NONE', *, *, #18093, .F. ) ;
#19623 = CARTESIAN_POINT ( 'NONE',  ( -40.00000000000000000, 19.00000000000000000, -26.00000000000000355 ) ) ;
#19624 = EDGE_LOOP ( 'NONE', ( #20334, #9096, #13476, #7209 ) ) ;
#19625 = LINE ( 'NONE', #5533, #794 ) ;
#19626 = EDGE_CURVE ( 'NONE', #1350, #17623, #18120, .T. ) ;
#19627 =( LENGTH_UNIT ( ) NAMED_UNIT ( * ) SI_UNIT ( .MILLI., .METRE. ) );
#19628 = SURFACE_STYLE_USAGE ( .BOTH. , #14715 ) ;
#19629 = LINE ( 'NONE', #3591, #12590 ) ;
#19630 = PLANE ( 'NONE',  #14790 ) ;
#19631 = PLANE ( 'NONE',  #17917 ) ;
#19632 = CARTESIAN_POINT ( 'NONE',  ( 1.469576158976824144E-15, 10.00000000000000000, 12.00000000000000178 ) ) ;
#19633 = CARTESIAN_POINT ( 'NONE',  ( 498.8334540492693918, 214.2156642432025251, 250.0000000000000000 ) ) ;
#19634 = DIRECTION ( 'NONE',  ( 0.000000000000000000, 1.000000000000000000, -0.000000000000000000 ) ) ;
#19635 = CARTESIAN_POINT ( 'NONE',  ( -23.00000000000003197, 3.000000000000000000, 34.00000000000000711 ) ) ;
#19636 = UNCERTAINTY_MEASURE_WITH_UNIT (LENGTH_MEASURE( 1.000000000000000082E-05 ), #9297, 'distance_accuracy_value', 'NONE');
#19637 = DIRECTION ( 'NONE',  ( -0.000000000000000000, -1.000000000000000000, -0.000000000000000000 ) ) ;
#19638 = ORIENTED_EDGE ( 'NONE', *, *, #18561, .T. ) ;
#19639 = EDGE_LOOP ( 'NONE', ( #3051, #14874, #18818, #3370 ) ) ;
#19640 = EDGE_CURVE ( 'NONE', #11794, #4707, #14956, .T. ) ;
#19641 = ORIENTED_EDGE ( 'NONE', *, *, #4607, .F. ) ;
#19642 = ORIENTED_EDGE ( 'NONE', *, *, #19443, .T. ) ;
#19643 = SURFACE_STYLE_USAGE ( .BOTH. , #13496 ) ;
#19644 = CARTESIAN_POINT ( 'NONE',  ( -20.00000000000003197, 3.000000000000000000, 40.00000000000000711 ) ) ;
#19645 = DIRECTION ( 'NONE',  ( 0.000000000000000000, -2.352167425053297897E-16, -1.000000000000000000 ) ) ;
#19646 = FACE_OUTER_BOUND ( 'NONE', #11198, .T. ) ;
#19647 = AXIS2_PLACEMENT_3D ( 'NONE', #6639, #19076, #17134 ) ;
#19648 = SURFACE_STYLE_FILL_AREA ( #14944 ) ;
#19649 = CARTESIAN_POINT ( 'NONE',  ( 3.674999999999999822, 14.43750000000000000, 0.000000000000000000 ) ) ;
#19651 = EDGE_CURVE ( 'NONE', #12704, #8671, #18233, .T. ) ;
#19650 = LINE ( 'NONE', #2839, #13358 ) ;
#19652 = VECTOR ( 'NONE', #17999, 1000.000000000000114 ) ;
#19653 = CARTESIAN_POINT ( 'NONE',  ( 40.00000000000000000, 68.00000000000000000, 26.00000000000000355 ) ) ;
#19654 = DIRECTION ( 'NONE',  ( 0.000000000000000000, 0.000000000000000000, -1.000000000000000000 ) ) ;
#19655 = DIRECTION ( 'NONE',  ( -0.000000000000000000, 1.000000000000000000, -0.000000000000000000 ) ) ;
#19656 = PRESENTATION_STYLE_ASSIGNMENT (( #1096 ) ) ;
#19657 = PRODUCT_DEFINITION ( 'UNKNOWN', '', #10610, #10284 ) ;
#19658 = CYLINDRICAL_SURFACE ( 'NONE', #1108, 3.000000000000002665 ) ;
#19659 = SURFACE_STYLE_USAGE ( .BOTH. , #10109 ) ;
#19660 = EDGE_CURVE ( 'NONE', #5074, #19976, #821, .T. ) ;
#19661 = EDGE_LOOP ( 'NONE', ( #3005, #14990, #19604, #6817 ) ) ;
#19662 = ORIENTED_EDGE ( 'NONE', *, *, #12538, .F. ) ;
#19663 = PRESENTATION_LAYER_ASSIGNMENT (  '', '', ( #6884 ) ) ;
#19664 = FACE_BOUND ( 'NONE', #18036, .T. ) ;
#19665 = ORIENTED_EDGE ( 'NONE', *, *, #5902, .F. ) ;
#19666 = EDGE_CURVE ( 'NONE', #19577, #17052, #14056, .T. ) ;
#19667 = ORIENTED_EDGE ( 'NONE', *, *, #568, .T. ) ;
#19668 = DIRECTION ( 'NONE',  ( -1.000000000000000000, 0.000000000000000000, -0.000000000000000000 ) ) ;
#19669 = FACE_OUTER_BOUND ( 'NONE', #18682, .T. ) ;
#19670 = ADVANCED_FACE ( 'NONE', ( #15619 ), #3327, .T. ) ;
#19672 = EDGE_CURVE ( 'NONE', #9566, #8826, #2455, .T. ) ;
#19671 = DIRECTION ( 'NONE',  ( 0.000000000000000000, 1.000000000000000000, 0.000000000000000000 ) ) ;
#19673 = CARTESIAN_POINT ( 'NONE',  ( 0.000000000000000000, 80.91625508013694912, 250.0000000000000000 ) ) ;
#19674 = FACE_BOUND ( 'NONE', #13265, .T. ) ;
#19675 = CARTESIAN_POINT ( 'NONE',  ( 78.48937290013660117, 123.1299228374914208, 170.4174721992565082 ) ) ;
#19676 = CARTESIAN_POINT ( 'NONE',  ( 31.00000000000003553, 0.000000000000000000, -22.99999999999999645 ) ) ;
#19677 = AXIS2_PLACEMENT_3D ( 'NONE', #9201, #10651, #16955 ) ;
#19678 = EDGE_CURVE ( 'NONE', #12591, #13473, #14491, .T. ) ;
#19679 = VERTEX_POINT ( 'NONE', #12605 ) ;
#19680 = DIRECTION ( 'NONE',  ( 1.000000000000000000, 0.000000000000000000, -3.854941057726247958E-16 ) ) ;
#19681 = CARTESIAN_POINT ( 'NONE',  ( -23.00000000000002487, 0.000000000000000000, -36.99999999999999289 ) ) ;
#19682 = LINE ( 'NONE', #16743, #17240 ) ;
#19683 = EDGE_CURVE ( 'NONE', #12618, #17973, #3133, .T. ) ;
#19684 = VERTEX_POINT ( 'NONE', #10960 ) ;
#19685 = EDGE_CURVE ( 'NONE', #9045, #12515, #17135, .T. ) ;
#19686 = ORIENTED_EDGE ( 'NONE', *, *, #17679, .T. ) ;
#19687 = AXIS2_PLACEMENT_3D ( 'NONE', #4645, #9173, #98 ) ;
#19688 = VECTOR ( 'NONE', #7644, 1000.000000000000000 ) ;
#19689 = EDGE_LOOP ( 'NONE', ( #11514, #13855, #5926, #8667 ) ) ;
#19690 = SURFACE_SIDE_STYLE ('',( #13452 ) ) ;
#19691 = PLANE ( 'NONE',  #6 ) ;
#19692 = EDGE_LOOP ( 'NONE', ( #197, #17474, #17339, #13774 ) ) ;
#19693 = LINE ( 'NONE', #5414, #4599 ) ;
#19694 = FACE_OUTER_BOUND ( 'NONE', #13607, .T. ) ;
#19695 = FACE_OUTER_BOUND ( 'NONE', #4697, .T. ) ;
#19697 = ADVANCED_FACE ( 'NONE', ( #1651 ), #9414, .T. ) ;
#19696 = CARTESIAN_POINT ( 'NONE',  ( -40.00000000000000711, 8.000000000000000000, -19.00000000000000355 ) ) ;
#19698 = UNCERTAINTY_MEASURE_WITH_UNIT (LENGTH_MEASURE( 1.000000000000000082E-05 ), #4693, 'distance_accuracy_value', 'NONE');
#19699 = CARTESIAN_POINT ( 'NONE',  ( -78.99999999999995737, 142.0976792249508946, 485.4122383872432351 ) ) ;
#19700 = DIRECTION ( 'NONE',  ( 0.000000000000000000, -0.000000000000000000, 1.000000000000000000 ) ) ;
#19701 = DIRECTION ( 'NONE',  ( 0.000000000000000000, 0.000000000000000000, 1.000000000000000000 ) ) ;
#19702 = APPLICATION_CONTEXT ( 'automotive_design' ) ;
#19703 = DIRECTION ( 'NONE',  ( -0.000000000000000000, -0.000000000000000000, 1.000000000000000000 ) ) ;
#19704 = CARTESIAN_POINT ( 'NONE',  ( -36.00000000000000711, 6.000000000000000000, -18.00000000000000355 ) ) ;
#19705 = AXIS2_PLACEMENT_3D ( 'NONE', #7110, #16191, #9784 ) ;
#19706 = MECHANICAL_DESIGN_GEOMETRIC_PRESENTATION_REPRESENTATION (  '', ( #12833 ), #2263 ) ;
#19707 = AXIS2_PLACEMENT_3D ( 'NONE', #16753, #6963, #13245 ) ;
#19708 = ORIENTED_EDGE ( 'NONE', *, *, #16807, .F. ) ;
#19709 = EDGE_CURVE ( 'NONE', #14517, #20017, #9598, .T. ) ;
#19710 = ORIENTED_EDGE ( 'NONE', *, *, #19223, .T. ) ;
#19711 = ORIENTED_EDGE ( 'NONE', *, *, #1737, .T. ) ;
#19712 = EDGE_CURVE ( 'NONE', #15985, #18686, #14165, .T. ) ;
#19713 = VERTEX_POINT ( 'NONE', #1763 ) ;
#19714 = EDGE_CURVE ( 'NONE', #3873, #1902, #8556, .T. ) ;
#19715 = DIRECTION ( 'NONE',  ( -0.000000000000000000, -0.000000000000000000, 1.000000000000000000 ) ) ;
#19716 = EDGE_LOOP ( 'NONE', ( #10446, #14679, #13852, #12852 ) ) ;
#19717 = FILL_AREA_STYLE ('',( #3000 ) ) ;
#19718 = DIRECTION ( 'NONE',  ( 1.000000000000000000, -0.000000000000000000, 0.000000000000000000 ) ) ;
#19719 =( GEOMETRIC_REPRESENTATION_CONTEXT ( 3 ) GLOBAL_UNCERTAINTY_ASSIGNED_CONTEXT ( ( #5380 ) ) GLOBAL_UNIT_ASSIGNED_CONTEXT ( ( #266, #14390, #12860 ) ) REPRESENTATION_CONTEXT ( 'NONE', 'WORKASPACE' ) );
#19720 = ORIENTED_EDGE ( 'NONE', *, *, #19252, .F. ) ;
#19721 = MECHANICAL_DESIGN_GEOMETRIC_PRESENTATION_REPRESENTATION (  '', ( #20044 ), #6928 ) ;
#19722 = PLANE ( 'NONE',  #3135 ) ;
#19723 = COLOUR_RGB ( '', 0.08235294, 0.09019608, 0.10196078) ;
#19724 = CARTESIAN_POINT ( 'NONE',  ( -31.00000000000002132, 10.00000000000000000, -31.00000000000000000 ) ) ;
#19725 = CARTESIAN_POINT ( 'NONE',  ( 0.2407302285477639081, 139.8437824378728180, 489.2196001188304990 ) ) ;
#19726 = CARTESIAN_POINT ( 'NONE',  ( 178.4893729001365728, 123.1299228374914918, 79.58252780074349175 ) ) ;
#19727 = FACE_OUTER_BOUND ( 'NONE', #16270, .T. ) ;
#19728 = SURFACE_STYLE_USAGE ( .BOTH. , #8257 ) ;
#19729 =( LENGTH_UNIT ( ) NAMED_UNIT ( * ) SI_UNIT ( .MILLI., .METRE. ) );
#19730 = LINE ( 'NONE', #1172, #1469 ) ;
#19731 = CARTESIAN_POINT ( 'NONE',  ( 111.4893729001366012, 129.7247684487574588, 370.0000000000000000 ) ) ;
#19732 = CARTESIAN_POINT ( 'NONE',  ( 0.000000000000000000, 66.00000000000000000, 0.000000000000000000 ) ) ;
#19733 = DIRECTION ( 'NONE',  ( -0.000000000000000000, -1.000000000000000000, -0.000000000000000000 ) ) ;
#19734 = CARTESIAN_POINT ( 'NONE',  ( 0.9999999999999876765, 216.7545334744432921, 501.8237260975781737 ) ) ;
#19735 = VERTEX_POINT ( 'NONE', #6438 ) ;
#19736 = AXIS2_PLACEMENT_3D ( 'NONE', #4530, #12949, #6189 ) ;
#19737 = CIRCLE ( 'NONE', #9219, 3.283624802691453848 ) ;
#19738 = VECTOR ( 'NONE', #8682, 1000.000000000000000 ) ;
#19739 = EDGE_CURVE ( 'NONE', #7970, #19399, #18583, .T. ) ;
#19740 = VECTOR ( 'NONE', #6524, 1000.000000000000000 ) ;
#19741 = LINE ( 'NONE', #4001, #13023 ) ;
#19742 = ORIENTED_EDGE ( 'NONE', *, *, #2217, .F. ) ;
#19743 = UNCERTAINTY_MEASURE_WITH_UNIT (LENGTH_MEASURE( 1.000000000000000082E-05 ), #11620, 'distance_accuracy_value', 'NONE');
#19744 = ORIENTED_EDGE ( 'NONE', *, *, #12487, .F. ) ;
#19745 = MECHANICAL_DESIGN_GEOMETRIC_PRESENTATION_REPRESENTATION (  '', ( #17123 ), #7278 ) ;
#19746 = ORIENTED_EDGE ( 'NONE', *, *, #10629, .F. ) ;
#19747 =( NAMED_UNIT ( * ) SI_UNIT ( $, .STERADIAN. ) SOLID_ANGLE_UNIT ( ) );
#19748 = PLANE ( 'NONE',  #11666 ) ;
#19749 = DIRECTION ( 'NONE',  ( 1.000000000000000000, 0.000000000000000000, -0.000000000000000000 ) ) ;
#19750 = FILL_AREA_STYLE ('',( #18323 ) ) ;
#19751 = DIRECTION ( 'NONE',  ( -1.000000000000000000, -0.000000000000000000, -0.000000000000000000 ) ) ;
#19752 = CONICAL_SURFACE ( 'NONE', #16495, 0.9999999999999950040, 1.029744258676644320 ) ;
#19753 = CARTESIAN_POINT ( 'NONE',  ( 109.4893729001365870, 211.0574367717017594, 346.4752554294135507 ) ) ;
#19754 = VECTOR ( 'NONE', #4972, 1000.000000000000000 ) ;
#19755 = CARTESIAN_POINT ( 'NONE',  ( -211.5106270998635409, 113.1299228374912502, 170.4174721992565082 ) ) ;
#19756 = DIRECTION ( 'NONE',  ( -0.000000000000000000, -0.000000000000000000, 1.000000000000000000 ) ) ;
#19757 = CARTESIAN_POINT ( 'NONE',  ( -79.99999999999995737, 140.0740644222055948, 488.6904065690556536 ) ) ;
#19758 = DIRECTION ( 'NONE',  ( -0.000000000000000000, -0.000000000000000000, 1.000000000000000000 ) ) ;
#19759 = DIRECTION ( 'NONE',  ( -0.000000000000000000, -1.000000000000000000, -0.000000000000000000 ) ) ;
#19760 = CARTESIAN_POINT ( 'NONE',  ( 10.00000000000000000, 381.0487089519832011, -80.00000000000332534 ) ) ;
#19761 =( NAMED_UNIT ( * ) PLANE_ANGLE_UNIT ( ) SI_UNIT ( $, .RADIAN. ) );
#19762 = EDGE_CURVE ( 'NONE', #15692, #16481, #9198, .T. ) ;
#19763 = AXIS2_PLACEMENT_3D ( 'NONE', #15684, #7826, #14316 ) ;
#19764 = VECTOR ( 'NONE', #12695, 1000.000000000000000 ) ;
#19765 = ORIENTED_EDGE ( 'NONE', *, *, #15648, .T. ) ;
#19766 = CARTESIAN_POINT ( 'NONE',  ( 10.00000000000000000, 306.0487089519832011, -80.00000000000380851 ) ) ;
#19767 = VERTEX_POINT ( 'NONE', #4571 ) ;
#19768 = ORIENTED_EDGE ( 'NONE', *, *, #10655, .T. ) ;
#19769 = CARTESIAN_POINT ( 'NONE',  ( -211.5106270998635409, 113.1299228374912502, 29.36128450348865471 ) ) ;
#19770 = UNCERTAINTY_MEASURE_WITH_UNIT (LENGTH_MEASURE( 1.000000000000000082E-05 ), #19505, 'distance_accuracy_value', 'NONE');
#19771 = CARTESIAN_POINT ( 'NONE',  ( 78.48937290013661539, 80.91625508013694912, 250.0000000000000000 ) ) ;
#19772 = DIRECTION ( 'NONE',  ( -0.000000000000000000, 1.000000000000000000, -0.000000000000000000 ) ) ;
#19773 =( NAMED_UNIT ( * ) SI_UNIT ( $, .STERADIAN. ) SOLID_ANGLE_UNIT ( ) );
#19774 = DIRECTION ( 'NONE',  ( -0.000000000000000000, -1.000000000000000000, -0.000000000000000000 ) ) ;
#19775 = DIRECTION ( 'NONE',  ( 0.000000000000000000, 0.000000000000000000, -1.000000000000000000 ) ) ;
#19776 = DIRECTION ( 'NONE',  ( 0.000000000000000000, 1.000000000000000000, 0.000000000000000000 ) ) ;
#19777 = EDGE_CURVE ( 'NONE', #15658, #6311, #6755, .T. ) ;
#19778 = PRESENTATION_LAYER_ASSIGNMENT (  '', '', ( #7956 ) ) ;
#19779 = FILL_AREA_STYLE ('',( #5582 ) ) ;
#19780 = DIRECTION ( 'NONE',  ( 0.000000000000000000, -0.000000000000000000, 1.000000000000000000 ) ) ;
#19781 = CARTESIAN_POINT ( 'NONE',  ( -81.00000000000136424, 138.8314847490560169, 489.5655098179835818 ) ) ;
#19782 = FACE_OUTER_BOUND ( 'NONE', #17665, .T. ) ;
#19783 = STYLED_ITEM ( 'NONE', ( #10798 ), #8611 ) ;
#19784 = ORIENTED_EDGE ( 'NONE', *, *, #1894, .T. ) ;
#19785 = DIRECTION ( 'NONE',  ( -9.815121534730717399E-17, 1.000000000000000000, 0.000000000000000000 ) ) ;
#19786 = CARTESIAN_POINT ( 'NONE',  ( -30.99999999999999289, 68.00000000000000000, 31.00000000000000000 ) ) ;
#19787 = CARTESIAN_POINT ( 'NONE',  ( 153.4893729001366580, 145.9162550801369491, -97.94896630388704750 ) ) ;
#19788 = ADVANCED_FACE ( 'NONE', ( #11256 ), #14758, .F. ) ;
#19789 = EDGE_LOOP ( 'NONE', ( #6496, #20326, #13451, #13359 ) ) ;
#19790 = UNCERTAINTY_MEASURE_WITH_UNIT (LENGTH_MEASURE( 1.000000000000000082E-05 ), #13701, 'distance_accuracy_value', 'NONE');
#19791 = EDGE_CURVE ( 'NONE', #4994, #15939, #14670, .T. ) ;
#19792 = ORIENTED_EDGE ( 'NONE', *, *, #7846, .T. ) ;
#19793 = DIRECTION ( 'NONE',  ( -0.000000000000000000, -0.000000000000000000, 1.000000000000000000 ) ) ;
#19794 = DIRECTION ( 'NONE',  ( 1.000000000000000000, 9.815121534730717399E-17, -0.000000000000000000 ) ) ;
#19795 = UNCERTAINTY_MEASURE_WITH_UNIT (LENGTH_MEASURE( 1.000000000000000082E-05 ), #15422, 'distance_accuracy_value', 'NONE');
#19796 = ORIENTED_EDGE ( 'NONE', *, *, #8834, .F. ) ;
#19797 = DIRECTION ( 'NONE',  ( 0.000000000000000000, 0.000000000000000000, 1.000000000000000000 ) ) ;
#19798 =( GEOMETRIC_REPRESENTATION_CONTEXT ( 3 ) GLOBAL_UNCERTAINTY_ASSIGNED_CONTEXT ( ( #4115 ) ) GLOBAL_UNIT_ASSIGNED_CONTEXT ( ( #17577, #11189, #6262 ) ) REPRESENTATION_CONTEXT ( 'NONE', 'WORKASPACE' ) );
#19799 = CARTESIAN_POINT ( 'NONE',  ( -1.274252908074454287E-14, 216.7545334744432921, 488.5655098179835818 ) ) ;
#19800 = VECTOR ( 'NONE', #14097, 1000.000000000000000 ) ;
#19801 = EDGE_CURVE ( 'NONE', #5105, #19851, #17119, .T. ) ;
#19802 = LINE ( 'NONE', #15095, #9398 ) ;
#19803 = CARTESIAN_POINT ( 'NONE',  ( -34.99999999999999289, 11.00000000000000000, 40.00000000000000711 ) ) ;
#19804 = STYLED_ITEM ( 'NONE', ( #988 ), #12075 ) ;
#19805 = ORIENTED_EDGE ( 'NONE', *, *, #17179, .T. ) ;
#19806 = FACE_OUTER_BOUND ( 'NONE', #6341, .T. ) ;
#19807 = EDGE_CURVE ( 'NONE', #13356, #14600, #9822, .T. ) ;
#19808 = VECTOR ( 'NONE', #12882, 1000.000000000000000 ) ;
#19809 = PRESENTATION_LAYER_ASSIGNMENT (  '', '', ( #3720 ) ) ;
#19810 = CARTESIAN_POINT ( 'NONE',  ( 25.99999999999996092, 0.000000000000000000, -33.99999999999998579 ) ) ;
#19811 = APPLICATION_PROTOCOL_DEFINITION ( 'draft international standard', 'automotive_design', 1998, #9860 ) ;
#19812 = ORIENTED_EDGE ( 'NONE', *, *, #13094, .F. ) ;
#19813 =( NAMED_UNIT ( * ) PLANE_ANGLE_UNIT ( ) SI_UNIT ( $, .RADIAN. ) );
#19814 = ORIENTED_EDGE ( 'NONE', *, *, #3344, .T. ) ;
#19815 = VERTEX_POINT ( 'NONE', #19298 ) ;
#19816 = PRODUCT_DEFINITION_FORMATION_WITH_SPECIFIED_SOURCE ( 'ANY', '', #9575, .NOT_KNOWN. ) ;
#19817 = EDGE_CURVE ( 'NONE', #19735, #14259, #8184, .T. ) ;
#19818 = VECTOR ( 'NONE', #5685, 1000.000000000000000 ) ;
#19819 = VERTEX_POINT ( 'NONE', #14454 ) ;
#19820 = CARTESIAN_POINT ( 'NONE',  ( 498.8334540492693918, 191.8198460455371333, 34.99421986894476788 ) ) ;
#19821 = ORIENTED_EDGE ( 'NONE', *, *, #10239, .F. ) ;
#19822 = DIRECTION ( 'NONE',  ( 9.815121534730717399E-17, -1.000000000000000000, 0.000000000000000000 ) ) ;
#19823 = AXIS2_PLACEMENT_3D ( 'NONE', #1263, #18619, #6466 ) ;
#19824 = DIRECTION ( 'NONE',  ( 0.000000000000000000, 0.000000000000000000, -1.000000000000000000 ) ) ;
#19825 = AXIS2_PLACEMENT_3D ( 'NONE', #15792, #7641, #7944 ) ;
#19826 = ORIENTED_EDGE ( 'NONE', *, *, #10065, .T. ) ;
#19827 = ADVANCED_FACE ( 'NONE', ( #8284 ), #14553, .T. ) ;
#19828 = LINE ( 'NONE', #7389, #10693 ) ;
#19829 = LINE ( 'NONE', #677, #8239 ) ;
#19830 = LINE ( 'NONE', #4097, #11603 ) ;
#19831 = ADVANCED_FACE ( 'NONE', ( #2267 ), #16342, .F. ) ;
#19832 = CARTESIAN_POINT ( 'NONE',  ( 5.945602903476760126, 13.89560290347679938, 0.000000000000000000 ) ) ;
#19833 = AXIS2_PLACEMENT_3D ( 'NONE', #11313, #378, #15576 ) ;
#19834 = DIRECTION ( 'NONE',  ( 1.000000000000000000, 5.889072920838430686E-16, -0.000000000000000000 ) ) ;
#19835 = DIRECTION ( 'NONE',  ( -0.000000000000000000, 1.000000000000000000, -0.000000000000000000 ) ) ;
#19836 = DIRECTION ( 'NONE',  ( -1.000000000000000000, -0.000000000000000000, -0.000000000000000000 ) ) ;
#19837 = DIRECTION ( 'NONE',  ( 0.000000000000000000, 0.000000000000000000, 1.000000000000000000 ) ) ;
#19838 = FILL_AREA_STYLE_COLOUR ( '', #13988 ) ;
#19839 = PLANE ( 'NONE',  #12940 ) ;
#19840 = LINE ( 'NONE', #13772, #12834 ) ;
#19841 = CARTESIAN_POINT ( 'NONE',  ( -40.00000000000000000, 68.00000000000000000, 26.00000000000000355 ) ) ;
#19842 =( NAMED_UNIT ( * ) PLANE_ANGLE_UNIT ( ) SI_UNIT ( $, .RADIAN. ) );
#19843 = VERTEX_POINT ( 'NONE', #11468 ) ;
#19844 = AXIS2_PLACEMENT_3D ( 'NONE', #13007, #5262, #8353 ) ;
#19845 = DIRECTION ( 'NONE',  ( 1.000000000000000000, 0.000000000000000000, 0.000000000000000000 ) ) ;
#19846 = EDGE_LOOP ( 'NONE', ( #10052, #9531, #3358, #4000 ) ) ;
#19847 = ORIENTED_EDGE ( 'NONE', *, *, #14433, .F. ) ;
#19848 = VECTOR ( 'NONE', #1790, 1000.000000000000000 ) ;
#19849 = COLOUR_RGB ( '', 0.72549020, 0.75294118, 0.79215686) ;
#19851 = VERTEX_POINT ( 'NONE', #727 ) ;
#19850 = EDGE_CURVE ( 'NONE', #16198, #11823, #17537, .T. ) ;
#19852 = AXIS2_PLACEMENT_3D ( 'NONE', #9942, #19401, #16152 ) ;
#19853 = CARTESIAN_POINT ( 'NONE',  ( -25.99999999999999645, 0.000000000000000000, -31.00000000000003197 ) ) ;
#19854 = CARTESIAN_POINT ( 'NONE',  ( -39.99999999999997868, 3.000000000000000000, -25.99999999999999645 ) ) ;
#19855 = CYLINDRICAL_SURFACE ( 'NONE', #11971, 3.299999999999997158 ) ;
#19856 = ADVANCED_FACE ( 'NONE', ( #434 ), #6947, .F. ) ;
#19857 = CARTESIAN_POINT ( 'NONE',  ( 53.48937290013659407, 209.4935875941501422, 345.2279431939882670 ) ) ;
#19858 = VECTOR ( 'NONE', #4042, 1000.000000000000000 ) ;
#19859 = CARTESIAN_POINT ( 'NONE',  ( 98.48937290013660117, 167.9162550801369491, 0.000000000000000000 ) ) ;
#19860 = VECTOR ( 'NONE', #3747, 1000.000000000000000 ) ;
#19861 = SURFACE_SIDE_STYLE ('',( #1835 ) ) ;
#19862 = FILL_AREA_STYLE_COLOUR ( '', #5677 ) ;
#19863 = SURFACE_SIDE_STYLE ('',( #10713 ) ) ;
#19864 = DIRECTION ( 'NONE',  ( 0.000000000000000000, 1.000000000000000000, -0.000000000000000000 ) ) ;
#19865 = DIRECTION ( 'NONE',  ( 0.000000000000000000, -0.7071067811865614505, -0.7071067811865336949 ) ) ;
#19866 = COLOUR_RGB ( '', 0.08235294, 0.09019608, 0.10196078) ;
#19867 = VECTOR ( 'NONE', #5957, 1000.000000000000000 ) ;
#19868 = CARTESIAN_POINT ( 'NONE',  ( -38.50085094405407204, 209.4098724938429541, 505.3921618609452935 ) ) ;
#19869 = FACE_OUTER_BOUND ( 'NONE', #6949, .T. ) ;
#19870 =( LENGTH_UNIT ( ) NAMED_UNIT ( * ) SI_UNIT ( .MILLI., .METRE. ) );
#19871 = VECTOR ( 'NONE', #7882, 1000.000000000000000 ) ;
#19872 = VECTOR ( 'NONE', #9030, 1000.000000000000000 ) ;
#19873 = VECTOR ( 'NONE', #11237, 1000.000000000000000 ) ;
#19874 =( GEOMETRIC_REPRESENTATION_CONTEXT ( 3 ) GLOBAL_UNCERTAINTY_ASSIGNED_CONTEXT ( ( #10113 ) ) GLOBAL_UNIT_ASSIGNED_CONTEXT ( ( #18578, #12292, #14999 ) ) REPRESENTATION_CONTEXT ( 'NONE', 'WORKASPACE' ) );
#19875 = VERTEX_POINT ( 'NONE', #2067 ) ;
#19876 = DIRECTION ( 'NONE',  ( 1.000000000000000000, 5.889072920838430686E-16, -0.000000000000000000 ) ) ;
#19877 = ORIENTED_EDGE ( 'NONE', *, *, #68, .T. ) ;
#19878 = ORIENTED_EDGE ( 'NONE', *, *, #17607, .F. ) ;
#19879 = CARTESIAN_POINT ( 'NONE',  ( -64.99999999999995737, 317.7545334744432353, 495.1946179577816451 ) ) ;
#19880 = PRESENTATION_STYLE_ASSIGNMENT (( #7537 ) ) ;
#19881 = DIRECTION ( 'NONE',  ( 0.000000000000000000, 1.000000000000000000, 0.000000000000000000 ) ) ;
#19882 = COLOUR_RGB ( '', 0.31764706, 0.68627451, 0.89019608) ;
#19883 = SURFACE_STYLE_FILL_AREA ( #1211 ) ;
#19884 = DIRECTION ( 'NONE',  ( 0.000000000000000000, 0.000000000000000000, -1.000000000000000000 ) ) ;
#19885 = EDGE_CURVE ( 'NONE', #8344, #4484, #13232, .T. ) ;
#19886 = DIRECTION ( 'NONE',  ( 1.000000000000000000, 0.000000000000000000, -0.000000000000000000 ) ) ;
#19887 = DIRECTION ( 'NONE',  ( 0.000000000000000000, -0.000000000000000000, 1.000000000000000000 ) ) ;
#19888 = CIRCLE ( 'NONE', #12331, 1.000000000000001110 ) ;
#19889 = MECHANICAL_DESIGN_GEOMETRIC_PRESENTATION_REPRESENTATION (  '', ( #4124 ), #14321 ) ;
#19890 = CYLINDRICAL_SURFACE ( 'NONE', #15297, 10.00000000000000888 ) ;
#19891 = CARTESIAN_POINT ( 'NONE',  ( 109.4893729001365870, 222.0013992467745823, 330.1364716053970483 ) ) ;
#19892 = FACE_OUTER_BOUND ( 'NONE', #15106, .T. ) ;
#19893 = AXIS2_PLACEMENT_3D ( 'NONE', #14947, #7495, #16979 ) ;
#19894 = LINE ( 'NONE', #1605, #64 ) ;
#19895 = ORIENTED_EDGE ( 'NONE', *, *, #10758, .T. ) ;
#19896 =( LENGTH_UNIT ( ) NAMED_UNIT ( * ) SI_UNIT ( .MILLI., .METRE. ) );
#19897 = FACE_BOUND ( 'NONE', #13807, .T. ) ;
#19898 = MECHANICAL_DESIGN_GEOMETRIC_PRESENTATION_REPRESENTATION (  '', ( #10054 ), #2781 ) ;
#19899 = CIRCLE ( 'NONE', #10695, 36.50000000000000000 ) ;
#19900 = VERTEX_POINT ( 'NONE', #13343 ) ;
#19901 = EDGE_CURVE ( 'NONE', #16181, #36, #16528, .T. ) ;
#19902 = CIRCLE ( 'NONE', #10063, 10.00000000000000888 ) ;
#19903 = VERTEX_POINT ( 'NONE', #5687 ) ;
#19904 = CARTESIAN_POINT ( 'NONE',  ( 35.00000000000000711, 19.00000000000000000, -21.00000000000000355 ) ) ;
#19905 = DIRECTION ( 'NONE',  ( 0.000000000000000000, 0.000000000000000000, 1.000000000000000000 ) ) ;
#19906 = ORIENTED_EDGE ( 'NONE', *, *, #13931, .T. ) ;
#19907 = DIRECTION ( 'NONE',  ( -0.000000000000000000, 1.000000000000000000, -0.000000000000000000 ) ) ;
#19908 = FILL_AREA_STYLE_COLOUR ( '', #10656 ) ;
#19909 = VECTOR ( 'NONE', #1756, 1000.000000000000000 ) ;
#19910 = LINE ( 'NONE', #4270, #14664 ) ;
#19911 = DIRECTION ( 'NONE',  ( 0.000000000000000000, 0.000000000000000000, 1.000000000000000000 ) ) ;
#19912 = EDGE_CURVE ( 'NONE', #3170, #17380, #10219, .T. ) ;
#19913 = FILL_AREA_STYLE ('',( #2406 ) ) ;
#19914 = ORIENTED_EDGE ( 'NONE', *, *, #9990, .T. ) ;
#19915 = DIRECTION ( 'NONE',  ( -1.000000000000000000, 0.000000000000000000, 7.715811803773179210E-14 ) ) ;
#19916 = CYLINDRICAL_SURFACE ( 'NONE', #18772, 1.000000000000015987 ) ;
#19917 = SHAPE_DEFINITION_REPRESENTATION ( #1307, #3934 ) ;
#19918 = ORIENTED_EDGE ( 'NONE', *, *, #17222, .F. ) ;
#19919 = ORIENTED_EDGE ( 'NONE', *, *, #10440, .F. ) ;
#19920 = ADVANCED_FACE ( 'NONE', ( #19892 ), #7580, .T. ) ;
#19921 = CARTESIAN_POINT ( 'NONE',  ( 133.4893729001365728, 167.9162550801369491, 0.000000000000000000 ) ) ;
#19922 = ORIENTED_EDGE ( 'NONE', *, *, #3563, .F. ) ;
#19923 = VERTEX_POINT ( 'NONE', #2379 ) ;
#19924 = AXIS2_PLACEMENT_3D ( 'NONE', #16921, #7635, #9088 ) ;
#19925 = ORIENTED_EDGE ( 'NONE', *, *, #14713, .T. ) ;
#19926 = DIRECTION ( 'NONE',  ( -0.000000000000000000, 1.000000000000000000, -0.000000000000000000 ) ) ;
#19927 = ORIENTED_EDGE ( 'NONE', *, *, #92, .F. ) ;
#19928 = DIRECTION ( 'NONE',  ( 0.000000000000000000, 0.000000000000000000, 1.000000000000000000 ) ) ;
#19929 = ADVANCED_FACE ( 'NONE', ( #14979 ), #2495, .F. ) ;
#19930 = CARTESIAN_POINT ( 'NONE',  ( 22.99999999999998224, 10.00000000000000000, 37.00000000000000711 ) ) ;
#19931 = ORIENTED_EDGE ( 'NONE', *, *, #9222, .F. ) ;
#19932 = FILL_AREA_STYLE_COLOUR ( '', #4679 ) ;
#19933 = DIRECTION ( 'NONE',  ( 5.540106248408141539E-14, 0.06294785233063035501, -0.9980168174369414835 ) ) ;
#19934 = FILL_AREA_STYLE_COLOUR ( '', #8320 ) ;
#19935 = EDGE_CURVE ( 'NONE', #6580, #13936, #19085, .T. ) ;
#19936 = CARTESIAN_POINT ( 'NONE',  ( -79.99999999999995737, 316.7545334744432353, 495.1946179577816451 ) ) ;
#19937 = DIRECTION ( 'NONE',  ( -0.000000000000000000, 1.000000000000000000, -0.000000000000000000 ) ) ;
#19938 = CARTESIAN_POINT ( 'NONE',  ( 111.4893729001366012, 127.7247684487574304, 250.0000000000000000 ) ) ;
#19939 = DIRECTION ( 'NONE',  ( 1.000000000000000000, 0.000000000000000000, 0.000000000000000000 ) ) ;
#19940 = CARTESIAN_POINT ( 'NONE',  ( -78.99999999999995737, 147.7545334744432921, 491.0690926367356042 ) ) ;
#19941 = SURFACE_STYLE_FILL_AREA ( #11932 ) ;
#19942 = LINE ( 'NONE', #9233, #6583 ) ;
#19943 = EDGE_CURVE ( 'NONE', #2567, #2417, #18255, .T. ) ;
#19944 = LINE ( 'NONE', #7594, #4328 ) ;
#19945 = LINE ( 'NONE', #10393, #7885 ) ;
#19946 = ORIENTED_EDGE ( 'NONE', *, *, #3467, .F. ) ;
#19947 = EDGE_CURVE ( 'NONE', #13170, #6967, #8574, .T. ) ;
#19948 = VERTEX_POINT ( 'NONE', #15385 ) ;
#19949 = EDGE_CURVE ( 'NONE', #7815, #3208, #13439, .T. ) ;
#19950 = ORIENTED_EDGE ( 'NONE', *, *, #9890, .T. ) ;
#19951 = VERTEX_POINT ( 'NONE', #19675 ) ;
#19952 = EDGE_CURVE ( 'NONE', #17171, #7013, #11882, .T. ) ;
#19953 = FACE_BOUND ( 'NONE', #1953, .T. ) ;
#19954 = ORIENTED_EDGE ( 'NONE', *, *, #18659, .F. ) ;
#19955 = CARTESIAN_POINT ( 'NONE',  ( 0.000000000000000000, 0.000000000000000000, 0.000000000000000000 ) ) ;
#19956 = PRESENTATION_STYLE_ASSIGNMENT (( #2856 ) ) ;
#19957 = CARTESIAN_POINT ( 'NONE',  ( -31.81980515339462912, 8.000000000000000000, -31.81980515339465043 ) ) ;
#19958 = VERTEX_POINT ( 'NONE', #15169 ) ;
#19959 = DIRECTION ( 'NONE',  ( 0.000000000000000000, 0.000000000000000000, -1.000000000000000000 ) ) ;
#19960 = DIRECTION ( 'NONE',  ( 1.000000000000000000, 5.889072920838430686E-16, -0.000000000000000000 ) ) ;
#19961 = PLANE ( 'NONE',  #3775 ) ;
#19962 = PLANE ( 'NONE',  #1742 ) ;
#19963 =( LENGTH_UNIT ( ) NAMED_UNIT ( * ) SI_UNIT ( .MILLI., .METRE. ) );
#19964 = CARTESIAN_POINT ( 'NONE',  ( -79.99999999999995737, 0.000000000000000000, 0.000000000000000000 ) ) ;
#19965 = DIRECTION ( 'NONE',  ( 0.000000000000000000, 0.000000000000000000, -1.000000000000000000 ) ) ;
#19966 = CARTESIAN_POINT ( 'NONE',  ( -81.18192946989275072, 216.7545334744432921, 499.8237260975782874 ) ) ;
#19967 = LINE ( 'NONE', #1195, #10561 ) ;
#19968 = PRESENTATION_LAYER_ASSIGNMENT (  '', '', ( #18331 ) ) ;
#19969 = FILL_AREA_STYLE_COLOUR ( '', #8725 ) ;
#19970 = ORIENTED_EDGE ( 'NONE', *, *, #4733, .T. ) ;
#19971 = EDGE_CURVE ( 'NONE', #19843, #19448, #1014, .T. ) ;
#19972 = EDGE_LOOP ( 'NONE', ( #3085, #12952 ) ) ;
#19973 = ORIENTED_EDGE ( 'NONE', *, *, #5231, .F. ) ;
#19974 = ADVANCED_FACE ( 'NONE', ( #10531 ), #5506, .T. ) ;
#19975 = DIRECTION ( 'NONE',  ( -1.000000000000000000, 0.000000000000000000, 0.000000000000000000 ) ) ;
#19976 = VERTEX_POINT ( 'NONE', #4986 ) ;
#19977 = VERTEX_POINT ( 'NONE', #2244 ) ;
#19978 = VECTOR ( 'NONE', #10852, 1000.000000000000000 ) ;
#19979 = PLANE ( 'NONE',  #4822 ) ;
#19980 = ADVANCED_FACE ( 'NONE', ( #4014 ), #7130, .T. ) ;
#19981 = FILL_AREA_STYLE_COLOUR ( '', #11302 ) ;
#19982 = UNCERTAINTY_MEASURE_WITH_UNIT (LENGTH_MEASURE( 1.000000000000000082E-05 ), #8059, 'distance_accuracy_value', 'NONE');
#19983 = CIRCLE ( 'NONE', #2557, 18.50000000000000000 ) ;
#19984 = CARTESIAN_POINT ( 'NONE',  ( 0.000000000000000000, 138.7723821175183048, 490.5025619656410640 ) ) ;
#19985 = DIRECTION ( 'NONE',  ( 0.000000000000000000, 0.000000000000000000, -1.000000000000000000 ) ) ;
#19986 = DIRECTION ( 'NONE',  ( 0.000000000000000000, 0.000000000000000000, -1.000000000000000000 ) ) ;
#19987 = LINE ( 'NONE', #11978, #9047 ) ;
#19988 = DIRECTION ( 'NONE',  ( 1.000000000000000000, 0.000000000000000000, 1.156482317317870344E-15 ) ) ;
#19989 = FACE_OUTER_BOUND ( 'NONE', #4307, .T. ) ;
#19990 = DIRECTION ( 'NONE',  ( 1.000000000000000000, 0.000000000000000000, -0.000000000000000000 ) ) ;
#19991 = CARTESIAN_POINT ( 'NONE',  ( -79.76822305802286905, 138.8141600818972847, 490.0314170930259934 ) ) ;
#19992 = EDGE_LOOP ( 'NONE', ( #12200, #3397, #12939, #8995 ) ) ;
#19993 = CARTESIAN_POINT ( 'NONE',  ( 40.00000000000001421, 3.000000000000000888, 0.000000000000000000 ) ) ;
#19994 =( LENGTH_UNIT ( ) NAMED_UNIT ( * ) SI_UNIT ( .MILLI., .METRE. ) );
#19995 = AXIS2_PLACEMENT_3D ( 'NONE', #14276, #3359, #14384 ) ;
#19996 = ADVANCED_FACE ( 'NONE', ( #17655 ), #7269, .F. ) ;
#19997 = EDGE_LOOP ( 'NONE', ( #19711, #10587, #9980, #9012 ) ) ;
#19998 = ORIENTED_EDGE ( 'NONE', *, *, #17555, .T. ) ;
#19999 = DIRECTION ( 'NONE',  ( 0.000000000000000000, 0.000000000000000000, -1.000000000000000000 ) ) ;
#20000 = CARTESIAN_POINT ( 'NONE',  ( -78.99999999999995737, 141.3905724437643414, 503.0282008302663144 ) ) ;
#20001 = EDGE_LOOP ( 'NONE', ( #19245, #14298, #3292, #14539 ) ) ;
#20002 = DIRECTION ( 'NONE',  ( -0.000000000000000000, -1.000000000000000000, -0.000000000000000000 ) ) ;
#20003 = PRESENTATION_STYLE_ASSIGNMENT (( #2705 ) ) ;
#20004 = DIRECTION ( 'NONE',  ( 1.000000000000000000, -0.000000000000000000, -0.000000000000000000 ) ) ;
#20005 = CARTESIAN_POINT ( 'NONE',  ( -80.65880741189570813, 140.4539905958026509, 500.8798623167376718 ) ) ;
#20006 = DIRECTION ( 'NONE',  ( 0.000000000000000000, 0.000000000000000000, -1.000000000000000000 ) ) ;
#20007 = ORIENTED_EDGE ( 'NONE', *, *, #13431, .T. ) ;
#20008 = FILL_AREA_STYLE_COLOUR ( '', #6935 ) ;
#20009 = DIRECTION ( 'NONE',  ( -1.000000000000000000, 0.000000000000000000, 0.000000000000000000 ) ) ;
#20010 = APPLICATION_PROTOCOL_DEFINITION ( 'draft international standard', 'automotive_design', 1998, #19331 ) ;
#20011 = VERTEX_POINT ( 'NONE', #10301 ) ;
#20012 = ORIENTED_EDGE ( 'NONE', *, *, #12710, .F. ) ;
#20013 = DIRECTION ( 'NONE',  ( 0.000000000000000000, 1.000000000000000000, 0.000000000000000000 ) ) ;
#20014 = ORIENTED_EDGE ( 'NONE', *, *, #9718, .T. ) ;
#20015 = VERTEX_POINT ( 'NONE', #331 ) ;
#20016 = MECHANICAL_DESIGN_GEOMETRIC_PRESENTATION_REPRESENTATION (  '', ( #18723 ), #14770 ) ;
#20017 = VERTEX_POINT ( 'NONE', #18023 ) ;
#20018 = CARTESIAN_POINT ( 'NONE',  ( 53.48937290013660828, 125.7247684487574304, 254.0000000000000000 ) ) ;
#20019 = EDGE_LOOP ( 'NONE', ( #16416, #8482, #14383, #16624, #8606, #4921 ) ) ;
#20020 = DIRECTION ( 'NONE',  ( 0.000000000000000000, 0.000000000000000000, 1.000000000000000000 ) ) ;
#20021 = PLANE ( 'NONE',  #13318 ) ;
#20022 = SURFACE_STYLE_FILL_AREA ( #18298 ) ;
#20023 = SURFACE_STYLE_FILL_AREA ( #13675 ) ;
#20024 = DIRECTION ( 'NONE',  ( 0.000000000000000000, 0.000000000000000000, 1.000000000000000000 ) ) ;
#20025 = STYLED_ITEM ( 'NONE', ( #383 ), #16227 ) ;
#20026 = FACE_OUTER_BOUND ( 'NONE', #15972, .T. ) ;
#20027 = CARTESIAN_POINT ( 'NONE',  ( 458.8334540492693350, 191.8198460455371333, 168.2339398819845826 ) ) ;
#20028 = CIRCLE ( 'NONE', #17413, 1.000000000000000888 ) ;
#20029 = CARTESIAN_POINT ( 'NONE',  ( -37.00000000000000711, 10.00000000000000000, -23.00000000000000000 ) ) ;
#20030 = AXIS2_PLACEMENT_3D ( 'NONE', #5821, #856, #2288 ) ;
#20031 = CARTESIAN_POINT ( 'NONE',  ( 133.4893729001365443, 123.1299228374914634, 220.6387154965113382 ) ) ;
#20032 =( GEOMETRIC_REPRESENTATION_CONTEXT ( 3 ) GLOBAL_UNCERTAINTY_ASSIGNED_CONTEXT ( ( #7174 ) ) GLOBAL_UNIT_ASSIGNED_CONTEXT ( ( #12636, #3356, #256 ) ) REPRESENTATION_CONTEXT ( 'NONE', 'WORKASPACE' ) );
#20033 = DIRECTION ( 'NONE',  ( 0.000000000000000000, 0.000000000000000000, -1.000000000000000000 ) ) ;
#20034 = EDGE_CURVE ( 'NONE', #18959, #20182, #10553, .T. ) ;
#20035 = PRESENTATION_STYLE_ASSIGNMENT (( #4208 ) ) ;
#20036 = DIRECTION ( 'NONE',  ( 1.000000000000000000, 0.000000000000000000, 0.000000000000000000 ) ) ;
#20037 = CARTESIAN_POINT ( 'NONE',  ( 30.90550859392619287, -64.11391548236646543, 66.87703344121223381 ) ) ;
#20038 = SURFACE_SIDE_STYLE ('',( #7199 ) ) ;
#20039 = SURFACE_STYLE_USAGE ( .BOTH. , #12128 ) ;
#20040 = FILL_AREA_STYLE_COLOUR ( '', #19053 ) ;
#20041 = CARTESIAN_POINT ( 'NONE',  ( 98.48937290013662960, 123.1299228374914350, 29.36128450348865471 ) ) ;
#20042 = FACE_OUTER_BOUND ( 'NONE', #2056, .T. ) ;
#20043 = AXIS2_PLACEMENT_3D ( 'NONE', #6676, #1897, #3576 ) ;
#20044 = STYLED_ITEM ( 'NONE', ( #15214 ), #6916 ) ;
#20045 = ORIENTED_EDGE ( 'NONE', *, *, #19935, .T. ) ;
#20046 = ADVANCED_FACE ( 'NONE', ( #1764 ), #9724, .F. ) ;
#20047 = AXIS2_PLACEMENT_3D ( 'NONE', #1134, #16539, #5509 ) ;
#20048 = ORIENTED_EDGE ( 'NONE', *, *, #6885, .T. ) ;
#20049 = LINE ( 'NONE', #13998, #7138 ) ;
#20050 = EDGE_LOOP ( 'NONE', ( #1225, #17858, #8960, #3161 ) ) ;
#20051 = LINE ( 'NONE', #15449, #5740 ) ;
#20052 = DIRECTION ( 'NONE',  ( 0.000000000000000000, -1.000000000000000000, 0.000000000000000000 ) ) ;
#20053 = FACE_OUTER_BOUND ( 'NONE', #14124, .T. ) ;
#20054 = EDGE_CURVE ( 'NONE', #9757, #6404, #16411, .T. ) ;
#20055 = VERTEX_POINT ( 'NONE', #13416 ) ;
#20056 = DIRECTION ( 'NONE',  ( 0.000000000000000000, 0.000000000000000000, -1.000000000000000000 ) ) ;
#20057 = FACE_OUTER_BOUND ( 'NONE', #8247, .T. ) ;
#20058 = ADVANCED_FACE ( 'NONE', ( #16038 ), #8080, .T. ) ;
#20059 = LINE ( 'NONE', #9252, #14317 ) ;
#20060 = CARTESIAN_POINT ( 'NONE',  ( 0.000000000000000000, 368.2663108437010919, -87.78239810828596035 ) ) ;
#20061 = CARTESIAN_POINT ( 'NONE',  ( 53.48937290013658696, 113.1299228374914065, 29.36128450348865471 ) ) ;
#20062 = AXIS2_PLACEMENT_3D ( 'NONE', #10302, #7433, #8768 ) ;
#20063 = DIRECTION ( 'NONE',  ( 1.000000000000000000, 0.000000000000000000, 0.000000000000000000 ) ) ;
#20064 = STYLED_ITEM ( 'NONE', ( #9525 ), #6993 ) ;
#20065 = LINE ( 'NONE', #817, #3654 ) ;
#20066 = AXIS2_PLACEMENT_3D ( 'NONE', #11760, #16503, #14950 ) ;
#20067 = AXIS2_PLACEMENT_3D ( 'NONE', #10211, #7146, #4340 ) ;
#20068 = CARTESIAN_POINT ( 'NONE',  ( -81.18192946989275072, 140.4048636633015406, 500.8237260975782874 ) ) ;
#20069 = DIRECTION ( 'NONE',  ( -1.000000000000000000, -0.000000000000000000, -0.000000000000000000 ) ) ;
#20070 = ADVANCED_FACE ( 'NONE', ( #16613 ), #2356, .F. ) ;
#20071 = ORIENTED_EDGE ( 'NONE', *, *, #11443, .T. ) ;
#20072 = ORIENTED_EDGE ( 'NONE', *, *, #4238, .F. ) ;
#20073 = VERTEX_POINT ( 'NONE', #6534 ) ;
#20074 = ORIENTED_EDGE ( 'NONE', *, *, #13216, .T. ) ;
#20075 = EDGE_CURVE ( 'NONE', #16481, #9564, #10640, .T. ) ;
#20076 = LINE ( 'NONE', #18535, #17587 ) ;
#20077 = ORIENTED_EDGE ( 'NONE', *, *, #3986, .F. ) ;
#20078 = ORIENTED_EDGE ( 'NONE', *, *, #14393, .F. ) ;
#20079 = DIRECTION ( 'NONE',  ( -1.000000000000000000, 0.000000000000000000, 0.000000000000000000 ) ) ;
#20080 = AXIS2_PLACEMENT_3D ( 'NONE', #8394, #17755, #3443 ) ;
#20081 = VECTOR ( 'NONE', #8471, 1000.000000000000000 ) ;
#20082 = AXIS2_PLACEMENT_3D ( 'NONE', #9672, #17490, #10921 ) ;
#20083 = CARTESIAN_POINT ( 'NONE',  ( 88.88953019741013861, 80.91625508013694912, 245.0000000000000000 ) ) ;
#20084 = LINE ( 'NONE', #19984, #12897 ) ;
#20085 = SURFACE_STYLE_USAGE ( .BOTH. , #2883 ) ;
#20086 = ADVANCED_FACE ( 'NONE', ( #9823 ), #18115, .F. ) ;
#20087 =( NAMED_UNIT ( * ) PLANE_ANGLE_UNIT ( ) SI_UNIT ( $, .RADIAN. ) );
#20088 = PRODUCT_DEFINITION_SHAPE ( 'NONE', 'NONE',  #1380 ) ;
#20089 = PLANE ( 'NONE',  #15603 ) ;
#20090 = VECTOR ( 'NONE', #14643, 1000.000000000000000 ) ;
#20091 = DIRECTION ( 'NONE',  ( 1.000000000000000000, 5.889072920838430686E-16, -0.000000000000000000 ) ) ;
#20092 = CARTESIAN_POINT ( 'NONE',  ( -26.00000000000002842, 0.000000000000000000, -31.00000000000003197 ) ) ;
#20093 = EDGE_CURVE ( 'NONE', #19149, #17151, #10972, .T. ) ;
#20094 = CARTESIAN_POINT ( 'NONE',  ( 39.99999999999999289, 10.00000000000000000, -26.00000000000000000 ) ) ;
#20095 = CARTESIAN_POINT ( 'NONE',  ( -1.000000000000012657, 140.6767719171587316, 502.2321032788613593 ) ) ;
#20096 = ORIENTED_EDGE ( 'NONE', *, *, #1682, .T. ) ;
#20097 = FACE_OUTER_BOUND ( 'NONE', #2164, .T. ) ;
#20098 =( NAMED_UNIT ( * ) SI_UNIT ( $, .STERADIAN. ) SOLID_ANGLE_UNIT ( ) );
#20099 = VECTOR ( 'NONE', #20173, 1000.000000000000000 ) ;
#20100 = DIRECTION ( 'NONE',  ( -1.000000000000000000, -0.000000000000000000, -0.000000000000000000 ) ) ;
#20101 = COLOUR_RGB ( '', 0.09019608, 0.27058824, 0.51372549) ;
#20102 = AXIS2_PLACEMENT_3D ( 'NONE', #7330, #7633, #5888 ) ;
#20103 = ORIENTED_EDGE ( 'NONE', *, *, #15716, .F. ) ;
#20104 =( REPRESENTATION_RELATIONSHIP ('NONE','NONE', #13279, #7605 ) REPRESENTATION_RELATIONSHIP_WITH_TRANSFORMATION ( #17661 )SHAPE_REPRESENTATION_RELATIONSHIP( ) );
#20105 = ORIENTED_EDGE ( 'NONE', *, *, #14033, .F. ) ;
#20106 = EDGE_CURVE ( 'NONE', #11813, #7140, #7220, .T. ) ;
#20107 = LINE ( 'NONE', #7654, #15980 ) ;
#20108 = VECTOR ( 'NONE', #7203, 1000.000000000000000 ) ;
#20109 = DIRECTION ( 'NONE',  ( 1.000000000000000000, 0.000000000000000000, 0.000000000000000000 ) ) ;
#20110 = ORIENTED_EDGE ( 'NONE', *, *, #14282, .F. ) ;
#20111 = DIRECTION ( 'NONE',  ( 0.000000000000000000, 1.000000000000000000, 0.000000000000000000 ) ) ;
#20112 = DIRECTION ( 'NONE',  ( 0.000000000000000000, 0.000000000000000000, 1.000000000000000000 ) ) ;
#20113 = LINE ( 'NONE', #7360, #17258 ) ;
#20114 = COLOUR_RGB ( '', 0.09019608, 0.27058824, 0.51372549) ;
#20115 = CARTESIAN_POINT ( 'NONE',  ( -80.82377052886815250, 140.4150287883843191, 500.8356803534629194 ) ) ;
#20116 = DIRECTION ( 'NONE',  ( 0.000000000000000000, 0.000000000000000000, -1.000000000000000000 ) ) ;
#20117 = CARTESIAN_POINT ( 'NONE',  ( 0.000000000000000000, 16.00000000000000000, -34.00000000000000000 ) ) ;
#20118 = VERTEX_POINT ( 'NONE', #12822 ) ;
#20119 = LINE ( 'NONE', #17050, #9907 ) ;
#20120 = SURFACE_SIDE_STYLE ('',( #2717 ) ) ;
#20121 = ORIENTED_EDGE ( 'NONE', *, *, #3532, .F. ) ;
#20122 = ORIENTED_EDGE ( 'NONE', *, *, #9374, .T. ) ;
#20123 = DIRECTION ( 'NONE',  ( 1.000000000000000000, 0.000000000000000000, 0.000000000000000000 ) ) ;
#20124 = ORIENTED_EDGE ( 'NONE', *, *, #3957, .F. ) ;
#20125 = AXIS2_PLACEMENT_3D ( 'NONE', #14560, #11380, #8289 ) ;
#20126 = EDGE_LOOP ( 'NONE', ( #15008, #544, #11848, #11869 ) ) ;
#20127 = ORIENTED_EDGE ( 'NONE', *, *, #15759, .F. ) ;
#20128 = DIRECTION ( 'NONE',  ( 1.000000000000000000, 0.000000000000000000, 0.000000000000000000 ) ) ;
#20129 = AXIS2_PLACEMENT_3D ( 'NONE', #8618, #3985, #13096 ) ;
#20130 = VERTEX_POINT ( 'NONE', #2865 ) ;
#20131 = DIRECTION ( 'NONE',  ( 1.156482317317881191E-15, 0.000000000000000000, 1.000000000000000000 ) ) ;
#20132 = CARTESIAN_POINT ( 'NONE',  ( 30.99999999999997868, 10.00000000000000000, -30.99999999999999645 ) ) ;
#20133 = AXIS2_PLACEMENT_3D ( 'NONE', #9952, #13253, #14784 ) ;
#20134 = CYLINDRICAL_SURFACE ( 'NONE', #2647, 2.000000000000001776 ) ;
#20135 = MECHANICAL_DESIGN_GEOMETRIC_PRESENTATION_REPRESENTATION (  '', ( #11942 ), #12593 ) ;
#20136 = DIRECTION ( 'NONE',  ( -0.000000000000000000, -1.000000000000000000, 0.000000000000000000 ) ) ;
#20137 = CARTESIAN_POINT ( 'NONE',  ( -79.99999999999995737, 152.4824555358010798, 501.3921618609452366 ) ) ;
#20138 = EDGE_CURVE ( 'NONE', #17493, #10815, #13606, .T. ) ;
#20139 =( NAMED_UNIT ( * ) SI_UNIT ( $, .STERADIAN. ) SOLID_ANGLE_UNIT ( ) );
#20140 = VECTOR ( 'NONE', #2196, 1000.000000000000000 ) ;
#20141 = CARTESIAN_POINT ( 'NONE',  ( -22.99999999999999645, 68.00000000000000000, 37.00000000000002132 ) ) ;
#20142 = CARTESIAN_POINT ( 'NONE',  ( 23.00000000000000711, 0.000000000000000000, -36.99999999999999289 ) ) ;
#20143 = CARTESIAN_POINT ( 'NONE',  ( 40.00000000000001421, 0.000000000000000000, -150.0000000000000000 ) ) ;
#20144 = DIRECTION ( 'NONE',  ( -6.982962677686266711E-15, 0.000000000000000000, -1.000000000000000000 ) ) ;
#20145 = LINE ( 'NONE', #18711, #13036 ) ;
#20146 = DIRECTION ( 'NONE',  ( 0.000000000000000000, 1.000000000000000000, 0.000000000000000000 ) ) ;
#20147 = DIRECTION ( 'NONE',  ( 0.000000000000000000, 1.000000000000000000, 0.000000000000000000 ) ) ;
#20148 = CIRCLE ( 'NONE', #11271, 2.500000000000002220 ) ;
#20149 =( LENGTH_UNIT ( ) NAMED_UNIT ( * ) SI_UNIT ( .MILLI., .METRE. ) );
#20150 = AXIS2_PLACEMENT_3D ( 'NONE', #10127, #11677, #3541 ) ;
#20151 = DIRECTION ( 'NONE',  ( 1.000000000000000000, 9.815121534730718631E-17, -0.000000000000000000 ) ) ;
#20152 = VERTEX_POINT ( 'NONE', #4231 ) ;
#20153 = CIRCLE ( 'NONE', #10299, 36.00000000000000000 ) ;
#20154 = VERTEX_POINT ( 'NONE', #7721 ) ;
#20155 = ORIENTED_EDGE ( 'NONE', *, *, #12709, .T. ) ;
#20156 = EDGE_CURVE ( 'NONE', #17182, #14898, #9320, .T. ) ;
#20157 = PRESENTATION_STYLE_ASSIGNMENT (( #4615 ) ) ;
#20158 = VERTEX_POINT ( 'NONE', #4422 ) ;
#20159 = LINE ( 'NONE', #9057, #12656 ) ;
#20160 = CARTESIAN_POINT ( 'NONE',  ( -21.00000000000002842, 0.000000000000000000, -34.99999999999999289 ) ) ;
#20161 = FILL_AREA_STYLE_COLOUR ( '', #1417 ) ;
#20162 = CLOSED_SHELL ( 'NONE', ( #4772, #5027, #20348, #15083, #6861, #3846, #13688 ) ) ;
#20163 = VECTOR ( 'NONE', #19191, 1000.000000000000000 ) ;
#20164 = EDGE_LOOP ( 'NONE', ( #5915, #19150, #19914, #15825 ) ) ;
#20165 = DIRECTION ( 'NONE',  ( -0.000000000000000000, 0.000000000000000000, 1.000000000000000000 ) ) ;
#20166 =( LENGTH_UNIT ( ) NAMED_UNIT ( * ) SI_UNIT ( .MILLI., .METRE. ) );
#20167 = DIRECTION ( 'NONE',  ( 0.000000000000000000, 0.000000000000000000, -1.000000000000000000 ) ) ;
#20168 = CARTESIAN_POINT ( 'NONE',  ( 111.4893729001366012, 127.7247684487574588, 254.0000000000000000 ) ) ;
#20169 =( LENGTH_UNIT ( ) NAMED_UNIT ( * ) SI_UNIT ( .MILLI., .METRE. ) );
#20170 = AXIS2_PLACEMENT_3D ( 'NONE', #18135, #5492, #19775 ) ;
#20171 = CARTESIAN_POINT ( 'NONE',  ( 53.48937290013658696, 103.1299228374913923, 220.6387154965113382 ) ) ;
#20172 = CARTESIAN_POINT ( 'NONE',  ( -21.00000000000002842, -20.00000000000000000, -34.99999999999999289 ) ) ;
#20173 = DIRECTION ( 'NONE',  ( 0.000000000000000000, 0.000000000000000000, -1.000000000000000000 ) ) ;
#20174 = EDGE_CURVE ( 'NONE', #3145, #19061, #15364, .T. ) ;
#20175 = SURFACE_STYLE_FILL_AREA ( #12251 ) ;
#20176 = SURFACE_STYLE_USAGE ( .BOTH. , #2564 ) ;
#20177 = VECTOR ( 'NONE', #2485, 1000.000000000000000 ) ;
#20178 = EDGE_CURVE ( 'NONE', #16867, #8912, #13893, .T. ) ;
#20179 = AXIS2_PLACEMENT_3D ( 'NONE', #20037, #12335, #18617 ) ;
#20180 = EDGE_LOOP ( 'NONE', ( #18809, #18405, #5504, #15667 ) ) ;
#20181 = EDGE_LOOP ( 'NONE', ( #14066, #18635, #1313, #855 ) ) ;
#20182 = VERTEX_POINT ( 'NONE', #2964 ) ;
#20183 = DIRECTION ( 'NONE',  ( 0.000000000000000000, 0.000000000000000000, 1.000000000000000000 ) ) ;
#20184 = ORIENTED_EDGE ( 'NONE', *, *, #1390, .F. ) ;
#20185 = EDGE_LOOP ( 'NONE', ( #17491, #12306, #4305, #11525 ) ) ;
#20186 = ORIENTED_EDGE ( 'NONE', *, *, #11662, .T. ) ;
#20187 = FACE_OUTER_BOUND ( 'NONE', #1653, .T. ) ;
#20188 = AXIS2_PLACEMENT_3D ( 'NONE', #20295, #17407, #8044 ) ;
#20189 = CARTESIAN_POINT ( 'NONE',  ( 53.48937290013660828, 34.32473510485366575, 250.0000000000000000 ) ) ;
#20190 = UNCERTAINTY_MEASURE_WITH_UNIT (LENGTH_MEASURE( 1.000000000000000082E-05 ), #864, 'distance_accuracy_value', 'NONE');
#20191 = CARTESIAN_POINT ( 'NONE',  ( 0.000000000000000000, 0.000000000000000000, 0.000000000000000000 ) ) ;
#20192 = ADVANCED_FACE ( 'NONE', ( #9255 ), #15459, .F. ) ;
#20193 = PLANE ( 'NONE',  #3651 ) ;
#20194 =( NAMED_UNIT ( * ) SI_UNIT ( $, .STERADIAN. ) SOLID_ANGLE_UNIT ( ) );
#20195 = PRESENTATION_LAYER_ASSIGNMENT (  '', '', ( #15285 ) ) ;
#20196 = CARTESIAN_POINT ( 'NONE',  ( -22.00000000000001776, 10.00000000000000000, 36.00000000000000711 ) ) ;
#20197 = CARTESIAN_POINT ( 'NONE',  ( 0.9999999999998859801, 139.7733885855926133, 500.8237260975781737 ) ) ;
#20198 = CIRCLE ( 'NONE', #1083, 10.00000000000000888 ) ;
#20199 = DIRECTION ( 'NONE',  ( 0.000000000000000000, 1.000000000000000000, 0.000000000000000000 ) ) ;
#20200 = CARTESIAN_POINT ( 'NONE',  ( -18.00000000000001421, 10.00000000000000000, 40.00000000000000711 ) ) ;
#20201 = PLANE ( 'NONE',  #4711 ) ;
#20202 = EDGE_CURVE ( 'NONE', #243, #270, #2664, .T. ) ;
#20203 = ORIENTED_EDGE ( 'NONE', *, *, #300, .F. ) ;
#20204 = FACE_OUTER_BOUND ( 'NONE', #20180, .T. ) ;
#20205 = CARTESIAN_POINT ( 'NONE',  ( -26.00000000000000000, 19.00000000000000000, 40.00000000000001421 ) ) ;
#20206 = CIRCLE ( 'NONE', #12311, 4.999999999999997335 ) ;
#20207 = AXIS2_PLACEMENT_3D ( 'NONE', #14646, #12910, #6834 ) ;
#20208 = MECHANICAL_DESIGN_GEOMETRIC_PRESENTATION_REPRESENTATION (  '', ( #8702 ), #6752 ) ;
#20209 = ADVANCED_FACE ( 'NONE', ( #13600 ), #16800, .F. ) ;
#20210 = AXIS2_PLACEMENT_3D ( 'NONE', #4945, #6495, #19146 ) ;
#20211 = AXIS2_PLACEMENT_3D ( 'NONE', #14094, #3376, #19128 ) ;
#20212 = VERTEX_POINT ( 'NONE', #6188 ) ;
#20213 = EDGE_CURVE ( 'NONE', #18834, #6655, #9069, .T. ) ;
#20214 = DIRECTION ( 'NONE',  ( 0.000000000000000000, -1.000000000000000000, 0.000000000000000000 ) ) ;
#20215 = ORIENTED_EDGE ( 'NONE', *, *, #1601, .T. ) ;
#20216 = EDGE_CURVE ( 'NONE', #17281, #3677, #7614, .T. ) ;
#20217 = VECTOR ( 'NONE', #3440, 1000.000000000000000 ) ;
#20218 = DIRECTION ( 'NONE',  ( 1.000000000000000000, -0.000000000000000000, 0.000000000000000000 ) ) ;
#20219 = VECTOR ( 'NONE', #19283, 1000.000000000000000 ) ;
#20220 = VECTOR ( 'NONE', #9977, 1000.000000000000000 ) ;
#20221 = ORIENTED_EDGE ( 'NONE', *, *, #16058, .T. ) ;
#20222 = CARTESIAN_POINT ( 'NONE',  ( -25.99999999999999645, 68.00000000000000000, 40.00000000000002132 ) ) ;
#20223 = CARTESIAN_POINT ( 'NONE',  ( 17.99999999999998224, 6.000000000000000000, -35.99999999999999289 ) ) ;
#20224 = STYLED_ITEM ( 'NONE', ( #10604 ), #16080 ) ;
#20225 = DIRECTION ( 'NONE',  ( -0.000000000000000000, 1.000000000000000000, -0.000000000000000000 ) ) ;
#20226 = DIRECTION ( 'NONE',  ( 0.000000000000000000, 0.000000000000000000, -1.000000000000000000 ) ) ;
#20227 = VECTOR ( 'NONE', #10397, 1000.000000000000000 ) ;
#20228 = DIRECTION ( 'NONE',  ( -0.000000000000000000, -1.000000000000000000, -0.000000000000000000 ) ) ;
#20229 = CARTESIAN_POINT ( 'NONE',  ( -31.00000000000006395, 19.00000000000000000, 20.99999999999998934 ) ) ;
#20230 = VECTOR ( 'NONE', #15212, 1000.000000000000000 ) ;
#20231 = ORIENTED_EDGE ( 'NONE', *, *, #2158, .T. ) ;
#20232 = CARTESIAN_POINT ( 'NONE',  ( 3.324999999999999734, 0.000000000000000000, 0.000000000000000000 ) ) ;
#20233 = EDGE_LOOP ( 'NONE', ( #3658, #7967, #8221, #12861 ) ) ;
#20234 = LINE ( 'NONE', #32, #12541 ) ;
#20235 = FACE_OUTER_BOUND ( 'NONE', #14958, .T. ) ;
#20236 = CIRCLE ( 'NONE', #16649, 10.00000000000000888 ) ;
#20237 = EDGE_LOOP ( 'NONE', ( #15039, #907, #19217, #10639 ) ) ;
#20238 = ORIENTED_EDGE ( 'NONE', *, *, #9758, .F. ) ;
#20239 = CARTESIAN_POINT ( 'NONE',  ( 55.48937290013660117, 127.7247684487574588, 368.0000000000000000 ) ) ;
#20240 = COLOUR_RGB ( '', 0.72549020, 0.75294118, 0.79215686) ;
#20241 = EDGE_LOOP ( 'NONE', ( #16007, #4193, #852, #17688 ) ) ;
#20242 = VECTOR ( 'NONE', #56, 1000.000000000000000 ) ;
#20243 = VERTEX_POINT ( 'NONE', #20171 ) ;
#20244 = VECTOR ( 'NONE', #9632, 1000.000000000000000 ) ;
#20245 = ORIENTED_EDGE ( 'NONE', *, *, #3078, .T. ) ;
#20246 = EDGE_CURVE ( 'NONE', #296, #19843, #1744, .T. ) ;
#20247 = AXIS2_PLACEMENT_3D ( 'NONE', #722, #8476, #10214 ) ;
#20248 = DIRECTION ( 'NONE',  ( 0.000000000000000000, 0.000000000000000000, -1.000000000000000000 ) ) ;
#20249 = ORIENTED_EDGE ( 'NONE', *, *, #6881, .F. ) ;
#20250 = CARTESIAN_POINT ( 'NONE',  ( 0.9999999999998859801, 140.4048636633015406, 500.8237260975781737 ) ) ;
#20251 = EDGE_CURVE ( 'NONE', #13902, #6600, #6081, .T. ) ;
#20252 = VECTOR ( 'NONE', #10567, 1000.000000000000000 ) ;
#20253 = CARTESIAN_POINT ( 'NONE',  ( 31.00000000000006750, 8.000000000000000000, -21.00000000000000355 ) ) ;
#20254 = DIRECTION ( 'NONE',  ( -3.854941057726249437E-16, -0.000000000000000000, 1.000000000000000000 ) ) ;
#20255 = DIRECTION ( 'NONE',  ( 0.000000000000000000, 1.000000000000000000, 0.000000000000000000 ) ) ;
#20256 = DIRECTION ( 'NONE',  ( -0.000000000000000000, -1.000000000000000000, -0.000000000000000000 ) ) ;
#20257 = FACE_OUTER_BOUND ( 'NONE', #6040, .T. ) ;
#20258 = CARTESIAN_POINT ( 'NONE',  ( -31.00000000000003197, 68.00000000000000000, 26.00000000000000355 ) ) ;
#20259 = DIRECTION ( 'NONE',  ( 1.000000000000000000, 0.000000000000000000, 0.000000000000000000 ) ) ;
#20260 = DIRECTION ( 'NONE',  ( 1.000000000000000000, -0.000000000000000000, -0.000000000000000000 ) ) ;
#20261 = CYLINDRICAL_SURFACE ( 'NONE', #1377, 3.000000000000000000 ) ;
#20262 = AXIS2_PLACEMENT_3D ( 'NONE', #16521, #11670, #4036 ) ;
#20263 = SURFACE_STYLE_USAGE ( .BOTH. , #9539 ) ;
#20264 = ORIENTED_EDGE ( 'NONE', *, *, #1024, .F. ) ;
#20265 = CIRCLE ( 'NONE', #16674, 1.000000000000000888 ) ;
#20266 = ORIENTED_EDGE ( 'NONE', *, *, #12519, .T. ) ;
#20267 = ADVANCED_FACE ( 'NONE', ( #18641 ), #2561, .F. ) ;
#20268 = ORIENTED_EDGE ( 'NONE', *, *, #1503, .F. ) ;
#20269 = CARTESIAN_POINT ( 'NONE',  ( -79.08769456577726942, 139.0123798169321958, 488.9260675989677907 ) ) ;
#20270 = VECTOR ( 'NONE', #8649, 1000.000000000000000 ) ;
#20271 = CARTESIAN_POINT ( 'NONE',  ( 18.99999999999998224, 10.00000000000000000, -39.99999999999999289 ) ) ;
#20272 = PRESENTATION_STYLE_ASSIGNMENT (( #3058 ) ) ;
#20273 = ORIENTED_EDGE ( 'NONE', *, *, #10440, .T. ) ;
#20274 = DIRECTION ( 'NONE',  ( -1.000000000000000000, -9.815121534730717399E-17, 0.000000000000000000 ) ) ;
#20275 = AXIS2_PLACEMENT_3D ( 'NONE', #16011, #1842, #8248 ) ;
#20276 = DIRECTION ( 'NONE',  ( 1.000000000000000000, 5.889072920838430686E-16, -0.000000000000000000 ) ) ;
#20277 = CARTESIAN_POINT ( 'NONE',  ( -1.000000000000012434, 141.6406393683235194, 501.8237260975781737 ) ) ;
#20278 = FILL_AREA_STYLE_COLOUR ( '', #110 ) ;
#20279 = CARTESIAN_POINT ( 'NONE',  ( -44.50085094405410757, 209.4098724938429541, 505.3921618609452935 ) ) ;
#20280 = CARTESIAN_POINT ( 'NONE',  ( -41.50085094405407915, 175.4489062796178871, 505.3921618609452935 ) ) ;
#20281 = CARTESIAN_POINT ( 'NONE',  ( 55.48937290013659407, 209.7811923590224978, 348.0151256184570343 ) ) ;
#20282 = CARTESIAN_POINT ( 'NONE',  ( -26.00000000000002132, 0.000000000000000000, 40.00000000000000711 ) ) ;
#20283 = CARTESIAN_POINT ( 'NONE',  ( -40.00000000000000711, 10.00000000000000000, 26.00000000000000000 ) ) ;
#20284 = EDGE_LOOP ( 'NONE', ( #6886, #17715 ) ) ;
#20285 = ORIENTED_EDGE ( 'NONE', *, *, #6628, .F. ) ;
#20286 = AXIS2_PLACEMENT_3D ( 'NONE', #3679, #19718, #8731 ) ;
#20287 = VERTEX_POINT ( 'NONE', #14101 ) ;
#20288 = DIRECTION ( 'NONE',  ( -1.000000000000000000, 0.000000000000000000, -1.322948291343119651E-12 ) ) ;
#20289 = ORIENTED_EDGE ( 'NONE', *, *, #672, .T. ) ;
#20290 = ORIENTED_EDGE ( 'NONE', *, *, #15716, .T. ) ;
#20291 = ORIENTED_EDGE ( 'NONE', *, *, #16462, .T. ) ;
#20292 = CARTESIAN_POINT ( 'NONE',  ( -39.99999999999997868, 0.000000000000000000, -25.99999999999999645 ) ) ;
#20293 = PLANE ( 'NONE',  #9333 ) ;
#20294 = EDGE_CURVE ( 'NONE', #6864, #20055, #1064, .T. ) ;
#20295 = CARTESIAN_POINT ( 'NONE',  ( 0.000000000000000000, 0.000000000000000000, 0.000000000000000000 ) ) ;
#20296 = CARTESIAN_POINT ( 'NONE',  ( 0.000000000000000000, 0.000000000000000000, 0.000000000000000000 ) ) ;
#20297 = DIRECTION ( 'NONE',  ( 1.000000000000000000, 0.000000000000000000, -0.000000000000000000 ) ) ;
#20298 = DIRECTION ( 'NONE',  ( 0.9999937692730440641, 0.003530072958125829961, 0.000000000000000000 ) ) ;
#20299 = EDGE_CURVE ( 'NONE', #13854, #17453, #15773, .T. ) ;
#20300 = DIRECTION ( 'NONE',  ( 0.000000000000000000, -1.000000000000000000, 0.000000000000000000 ) ) ;
#20301 = DIRECTION ( 'NONE',  ( 0.000000000000000000, 0.000000000000000000, 1.000000000000000000 ) ) ;
#20302 = DIRECTION ( 'NONE',  ( 1.000000000000000000, -0.000000000000000000, -0.000000000000000000 ) ) ;
#20303 = CARTESIAN_POINT ( 'NONE',  ( -20.99999999999999645, 8.000000000000000000, 35.00000000000001421 ) ) ;
#20304 = ORIENTED_EDGE ( 'NONE', *, *, #14720, .F. ) ;
#20305 = DIRECTION ( 'NONE',  ( -1.000000000000000000, -1.595148023886719315E-16, 0.000000000000000000 ) ) ;
#20306 = DIRECTION ( 'NONE',  ( 0.000000000000000000, 0.000000000000000000, -1.000000000000000000 ) ) ;
#20307 = EDGE_CURVE ( 'NONE', #1465, #625, #9655, .T. ) ;
#20308 = LINE ( 'NONE', #1318, #17599 ) ;
#20309 = ORIENTED_EDGE ( 'NONE', *, *, #5012, .T. ) ;
#20310 = EDGE_CURVE ( 'NONE', #15658, #4273, #4057, .T. ) ;
#20311 = ADVANCED_FACE ( 'NONE', ( #6285 ), #15935, .T. ) ;
#20312 = DIRECTION ( 'NONE',  ( 1.000000000000000000, 9.815121534730717399E-17, -0.000000000000000000 ) ) ;
#20313 = EDGE_LOOP ( 'NONE', ( #7073, #11991, #16594, #11453 ) ) ;
#20314 = DIRECTION ( 'NONE',  ( 0.000000000000000000, 0.000000000000000000, 1.000000000000000000 ) ) ;
#20315 =( LENGTH_UNIT ( ) NAMED_UNIT ( * ) SI_UNIT ( .MILLI., .METRE. ) );
#20316 = EDGE_LOOP ( 'NONE', ( #20330, #4520, #8178, #271, #16465 ) ) ;
#20317 =( LENGTH_UNIT ( ) NAMED_UNIT ( * ) SI_UNIT ( .MILLI., .METRE. ) );
#20318 = CARTESIAN_POINT ( 'NONE',  ( 82.88953019741013861, 80.91625508013694912, 245.0000000000000000 ) ) ;
#20319 = FILL_AREA_STYLE_COLOUR ( '', #3124 ) ;
#20320 = ADVANCED_FACE ( 'NONE', ( #1604 ), #17301, .T. ) ;
#20321 = FACE_BOUND ( 'NONE', #11384, .T. ) ;
#20322 = EDGE_CURVE ( 'NONE', #584, #16123, #3281, .T. ) ;
#20323 = CARTESIAN_POINT ( 'NONE',  ( 10.00000000000000000, 301.0487089519826327, 2.148629195649657075E-12 ) ) ;
#20324 = CARTESIAN_POINT ( 'NONE',  ( -31.00000000000002842, 3.000000000000000000, 31.00000000000000000 ) ) ;
#20325 = AXIS2_PLACEMENT_3D ( 'NONE', #3183, #15872, #18935 ) ;
#20326 = ORIENTED_EDGE ( 'NONE', *, *, #9494, .F. ) ;
#20327 = DIRECTION ( 'NONE',  ( 0.000000000000000000, 1.000000000000000000, 0.000000000000000000 ) ) ;
#20328 = PLANE ( 'NONE',  #6623 ) ;
#20329 = CONTEXT_DEPENDENT_SHAPE_REPRESENTATION ( #1818, #1848 ) ;
#20330 = ORIENTED_EDGE ( 'NONE', *, *, #4374, .T. ) ;
#20331 = DIRECTION ( 'NONE',  ( 2.775557561562888827E-14, 0.000000000000000000, -1.000000000000000000 ) ) ;
#20332 = EDGE_CURVE ( 'NONE', #4114, #6573, #12987, .T. ) ;
#20333 = ORIENTED_EDGE ( 'NONE', *, *, #12282, .T. ) ;
#20334 = ORIENTED_EDGE ( 'NONE', *, *, #2817, .F. ) ;
#20335 = ORIENTED_EDGE ( 'NONE', *, *, #1404, .T. ) ;
#20336 = EDGE_CURVE ( 'NONE', #9458, #10589, #7920, .T. ) ;
#20337 = AXIS2_PLACEMENT_3D ( 'NONE', #4906, #18799, #7893 ) ;
#20338 = ORIENTED_EDGE ( 'NONE', *, *, #20294, .T. ) ;
#20339 = DIRECTION ( 'NONE',  ( -0.000000000000000000, 1.000000000000000000, -0.000000000000000000 ) ) ;
#20340 = PRESENTATION_STYLE_ASSIGNMENT (( #1673 ) ) ;
#20341 =( NAMED_UNIT ( * ) PLANE_ANGLE_UNIT ( ) SI_UNIT ( $, .RADIAN. ) );
#20342 = DIRECTION ( 'NONE',  ( 1.000000000000000000, 0.000000000000000000, 0.000000000000000000 ) ) ;
#20343 =( NAMED_UNIT ( * ) PLANE_ANGLE_UNIT ( ) SI_UNIT ( $, .RADIAN. ) );
#20344 = CARTESIAN_POINT ( 'NONE',  ( 0.3499999999999999778, 0.000000000000000000, 0.000000000000000000 ) ) ;
#20345 = DIRECTION ( 'NONE',  ( 0.000000000000000000, 0.000000000000000000, -1.000000000000000000 ) ) ;
#20346 = ORIENTED_EDGE ( 'NONE', *, *, #1476, .F. ) ;
#20347 = CYLINDRICAL_SURFACE ( 'NONE', #6536, 17.52499999999999858 ) ;
#20348 = ADVANCED_FACE ( 'NONE', ( #14202 ), #19022, .T. ) ;
#20349 = LINE ( 'NONE', #17464, #2036 ) ;
#20350 = DIRECTION ( 'NONE',  ( -1.135258727068399668E-15, 0.000000000000000000, 1.000000000000000000 ) ) ;
#20351 = FACE_OUTER_BOUND ( 'NONE', #7164, .T. ) ;
#20352 = STYLED_ITEM ( 'NONE', ( #16760 ), #4856 ) ;
#20353 = CARTESIAN_POINT ( 'NONE',  ( 153.4893729001366580, 145.9162550801369491, 250.0000000000000000 ) ) ;
#20354 = PRESENTATION_STYLE_ASSIGNMENT (( #6366 ) ) ;
#20355 = VERTEX_POINT ( 'NONE', #78 ) ;
#20356 = ADVANCED_FACE ( 'NONE', ( #4626 ), #14408, .F. ) ;
#20357 = ORIENTED_EDGE ( 'NONE', *, *, #10266, .F. ) ;
#20358 = ORIENTED_EDGE ( 'NONE', *, *, #20093, .F. ) ;
#20359 = ORIENTED_EDGE ( 'NONE', *, *, #8750, .F. ) ;
#20360 = FACE_OUTER_BOUND ( 'NONE', #8844, .T. ) ;
#20361 = CARTESIAN_POINT ( 'NONE',  ( -80.45802087912527156, 140.5471886258677614, 500.9805408940079019 ) ) ;
#20362 = EDGE_LOOP ( 'NONE', ( #4118, #18734, #12738, #10373 ) ) ;
#20363 = COLOUR_RGB ( '', 0.09019608, 0.27058824, 0.51372549) ;
#20364 = VECTOR ( 'NONE', #10837, 1000.000000000000000 ) ;
#20365 = DIRECTION ( 'NONE',  ( 1.000000000000000000, 9.815121534730718631E-17, -0.000000000000000000 ) ) ;
#20366 = CIRCLE ( 'NONE', #11499, 1.000000000000000888 ) ;
#20367 = VERTEX_POINT ( 'NONE', #14505 ) ;
#20368 = FACE_OUTER_BOUND ( 'NONE', #17308, .T. ) ;
#20369 = DIRECTION ( 'NONE',  ( -0.000000000000000000, -1.000000000000000000, -0.000000000000000000 ) ) ;
#20370 = CARTESIAN_POINT ( 'NONE',  ( 1.181929469892549101, 147.7545334744432921, 491.0690926367356042 ) ) ;
#20371 = LINE ( 'NONE', #17088, #1747 ) ;
#20372 = DIRECTION ( 'NONE',  ( 0.000000000000000000, 1.000000000000000000, 0.000000000000000000 ) ) ;
#20373 = NEXT_ASSEMBLY_USAGE_OCCURRENCE ( 'NAUO1', ' ', ' ', #14255, #14766, $ ) ;
#20374 = NEXT_ASSEMBLY_USAGE_OCCURRENCE ( 'NAUO2', ' ', ' ', #14255, #1380, $ ) ;
#20375 = NEXT_ASSEMBLY_USAGE_OCCURRENCE ( 'NAUO3', ' ', ' ', #14255, #15412, $ ) ;
#20376 = NEXT_ASSEMBLY_USAGE_OCCURRENCE ( 'NAUO4', ' ', ' ', #14255, #8109, $ ) ;
#20377 = NEXT_ASSEMBLY_USAGE_OCCURRENCE ( 'NAUO5', ' ', ' ', #14255, #5698, $ ) ;
#20378 = NEXT_ASSEMBLY_USAGE_OCCURRENCE ( 'NAUO6', ' ', ' ', #14255, #13881, $ ) ;
#20379 = NEXT_ASSEMBLY_USAGE_OCCURRENCE ( 'NAUO7', ' ', ' ', #14255, #9349, $ ) ;
#20380 = NEXT_ASSEMBLY_USAGE_OCCURRENCE ( 'NAUO8', ' ', ' ', #14255, #1129, $ ) ;
#20381 = NEXT_ASSEMBLY_USAGE_OCCURRENCE ( 'NAUO9', ' ', ' ', #14766, #15789, $ ) ;
#20382 = NEXT_ASSEMBLY_USAGE_OCCURRENCE ( 'NAUO10', ' ', ' ', #14766, #17285, $ ) ;
#20383 = NEXT_ASSEMBLY_USAGE_OCCURRENCE ( 'NAUO11', ' ', ' ', #14766, #13275, $ ) ;
#20384 = NEXT_ASSEMBLY_USAGE_OCCURRENCE ( 'NAUO12', ' ', ' ', #14766, #158, $ ) ;
#20385 = NEXT_ASSEMBLY_USAGE_OCCURRENCE ( 'NAUO13', ' ', ' ', #14766, #2914, $ ) ;
#20386 = NEXT_ASSEMBLY_USAGE_OCCURRENCE ( 'NAUO14', ' ', ' ', #14766, #7839, $ ) ;
#20387 = NEXT_ASSEMBLY_USAGE_OCCURRENCE ( 'NAUO15', ' ', ' ', #14766, #19657, $ ) ;
ENDSEC;
END-ISO-10303-21;
